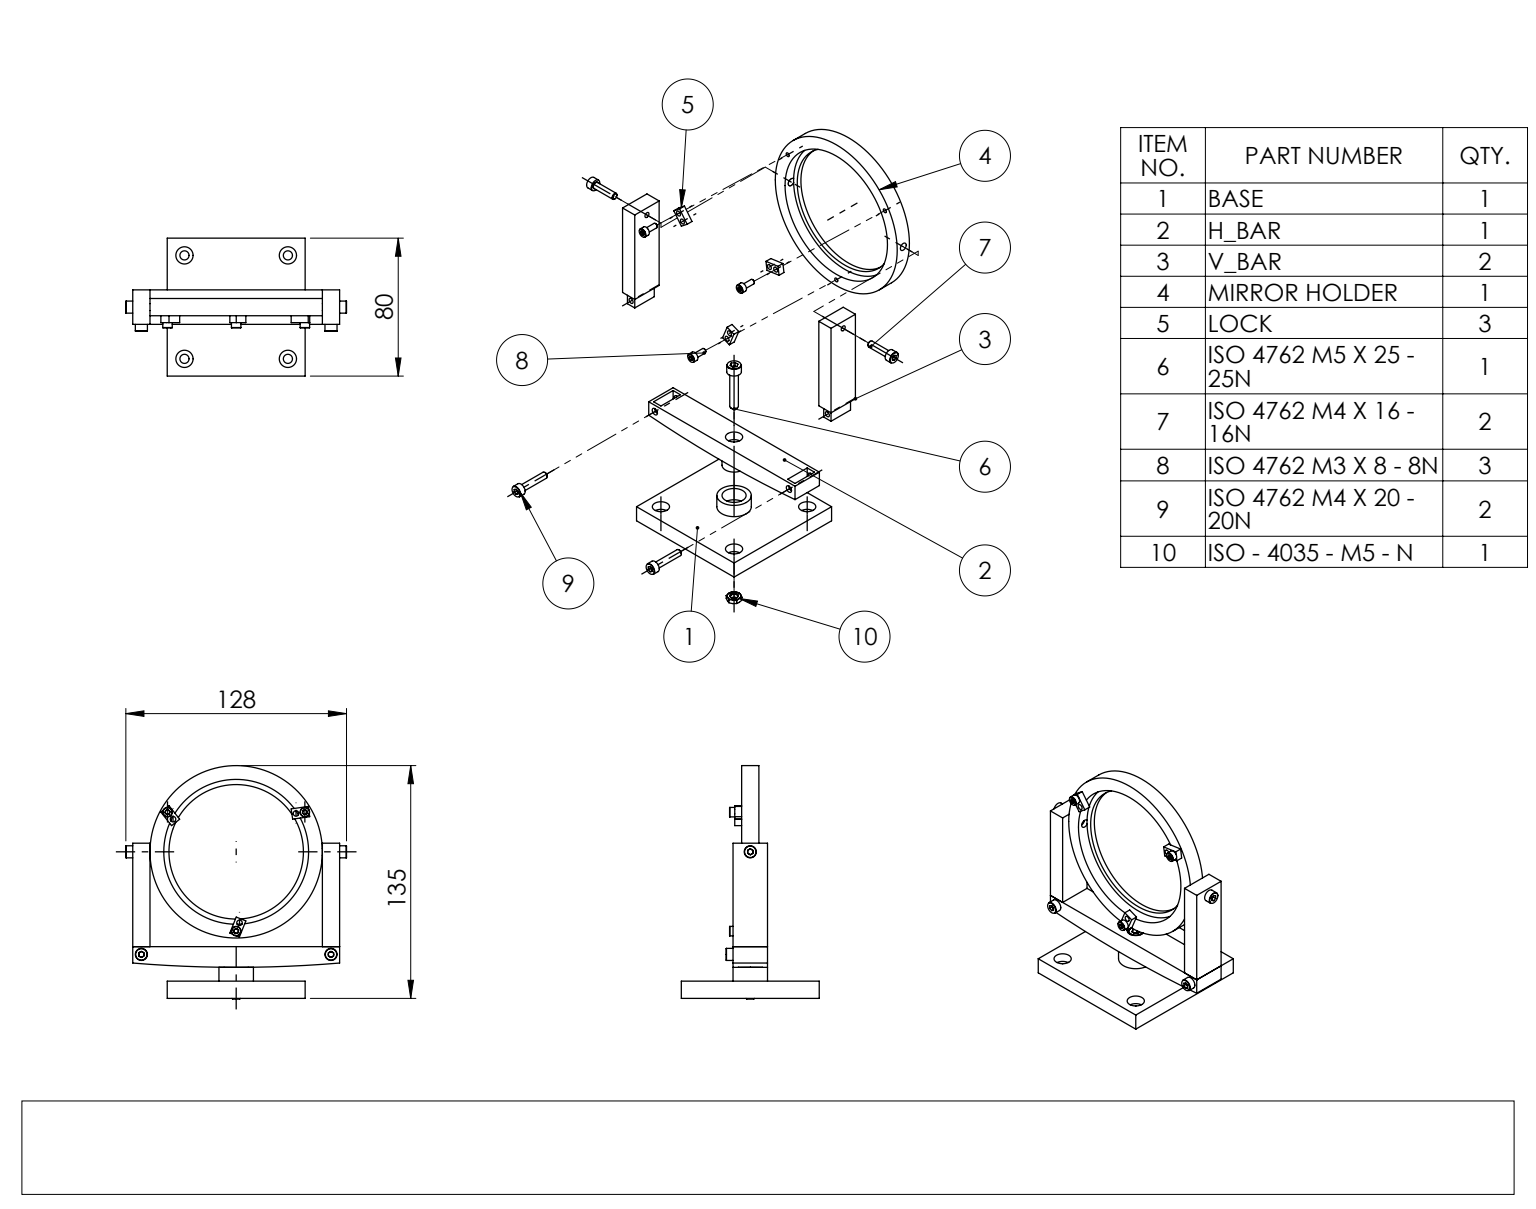
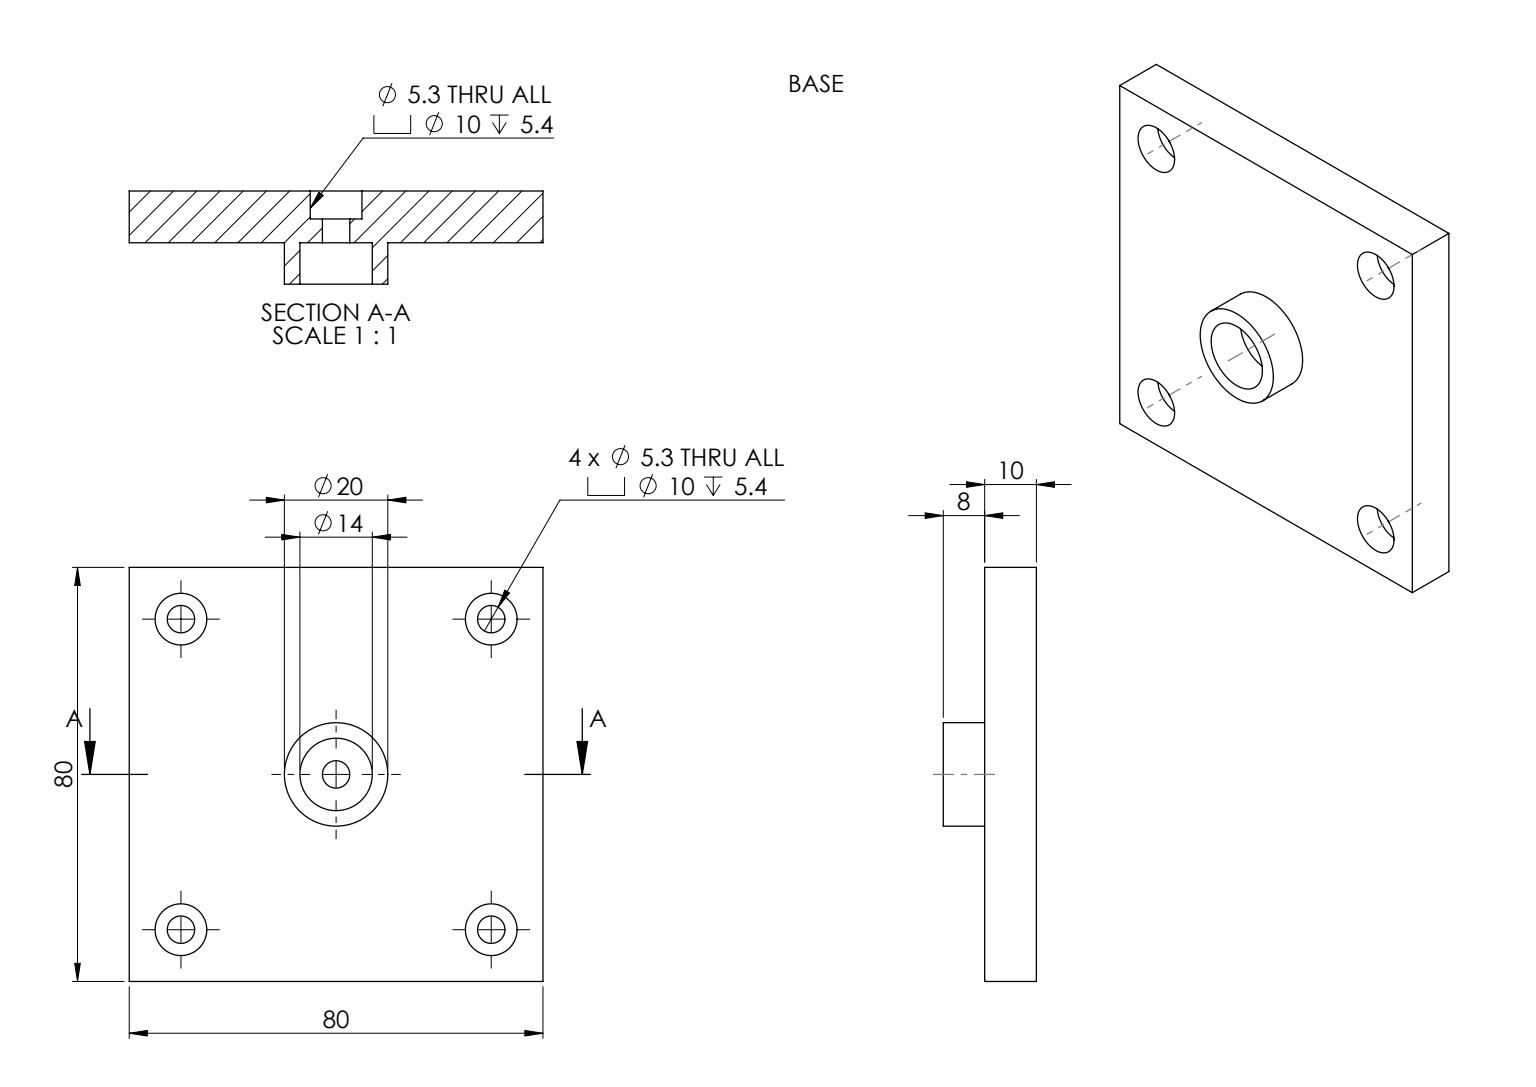
ISO-10303-21;
HEADER;
FILE_DESCRIPTION (('STEP AP214'),
    '1' );
FILE_NAME ('BR-153',
    '2026-10-08T12:12:07',
    ( '' ),
    ( '' ),
    'SwSTEP 2.0',
    'SolidWorks 2026',
    '' );
FILE_SCHEMA (( 'AUTOMOTIVE_DESIGN' ));
ENDSEC;

DATA;
#1 = ORIENTED_EDGE ( 'NONE', *, *, #482, .T. ) ;
#2 = DIRECTION ( 'NONE',  ( -0.000000000000000000, -0.000000000000000000, -1.000000000000000000 ) ) ;
#3 = ORIENTED_EDGE ( 'NONE', *, *, #6998, .T. ) ;
#4 = ORIENTED_EDGE ( 'NONE', *, *, #3995, .T. ) ;
#5 = PRODUCT_DEFINITION_SHAPE ( 'NONE', 'NONE',  #2283 ) ;
#6 = DIRECTION ( 'NONE',  ( -1.000000000000000000, 0.000000000000000000, 0.000000000000000000 ) ) ;
#7 = CARTESIAN_POINT ( 'NONE',  ( -34.99999999999999289, 30.00000000000000711, 10.00000000000000000 ) ) ;
#8 = CARTESIAN_POINT ( 'NONE',  ( 11.00000000000000355, 0.000000000000000000, 1.219500000000000028 ) ) ;
#9 = ADVANCED_BREP_SHAPE_REPRESENTATION ( '', ( #3934, #1587 ), #3111 ) ;
#10 = DIRECTION ( 'NONE',  ( 0.6609621790636541760, 0.7504192147376197441, -8.448647189793598288E-19 ) ) ;
#11 = CIRCLE ( 'NONE', #4655, 3.299999999999999822 ) ;
#12 = B_SPLINE_CURVE_WITH_KNOTS ( 'NONE', 3,
 ( #534, #1149, #5570, #2945, #3074, #6720 ),
 .UNSPECIFIED., .F., .F.,
 ( 4, 2, 4 ),
 ( 0.006456566858647395761, 0.007625406818786665576, 0.008794246778925936259 ),
 .UNSPECIFIED. ) ;
#13 = ORIENTED_EDGE ( 'NONE', *, *, #1918, .T. ) ;
#14 = CARTESIAN_POINT ( 'NONE',  ( 49.97494079589864668, 83.41331875350536507, -1.807471472119508205 ) ) ;
#15 = ORIENTED_EDGE ( 'NONE', *, *, #6393, .F. ) ;
#16 = EDGE_LOOP ( 'NONE', ( #282, #7065, #6159, #322 ) ) ;
#17 = ADVANCED_FACE ( 'NONE', ( #5328 ), #856, .F. ) ;
#18 = CARTESIAN_POINT ( 'NONE',  ( -10.00000000000000000, 0.000000000000000000, 18.00000000000000355 ) ) ;
#19 = CARTESIAN_POINT ( 'NONE',  ( 42.00000000000004263, 84.74554347572708934, -2.399999999999959943 ) ) ;
#20 = DIRECTION ( 'NONE',  ( 0.8191520442889896891, 1.003171929053522158E-16, -0.5735764363510490460 ) ) ;
#21 =( LENGTH_UNIT ( ) NAMED_UNIT ( * ) SI_UNIT ( .MILLI., .METRE. ) );
#22 = CYLINDRICAL_SURFACE ( 'NONE', #7576, 2.399999999999985256 ) ;
#23 = ORIENTED_EDGE ( 'NONE', *, *, #1900, .T. ) ;
#24 = ADVANCED_FACE ( 'NONE', ( #2123 ), #1462, .F. ) ;
#25 = CARTESIAN_POINT ( 'NONE',  ( 0.000000000000000000, 0.000000000000000000, 0.000000000000000000 ) ) ;
#26 = CARTESIAN_POINT ( 'NONE',  ( 0.1999999999999987899, 0.000000000000000000, 0.000000000000000000 ) ) ;
#27 = CARTESIAN_POINT ( 'NONE',  ( 29.99999999999997868, 30.00000000000001421, 10.00000000000000000 ) ) ;
#28 = CARTESIAN_POINT ( 'NONE',  ( 1.300000000000000044, 1.478016689125442484, -1.626303258728256651E-15 ) ) ;
#29 = DIRECTION ( 'NONE',  ( 1.000000000000000000, 0.000000000000000000, 0.000000000000000000 ) ) ;
#30 = CARTESIAN_POINT ( 'NONE',  ( 29.99999999999997868, 30.00000000000001421, 10.00000000000000000 ) ) ;
#31 = VECTOR ( 'NONE', #6228, 1000.000000000000000 ) ;
#32 = EDGE_LOOP ( 'NONE', ( #2251, #1109, #2656, #3323 ) ) ;
#33 = EDGE_CURVE ( 'NONE', #5370, #4266, #4037, .T. ) ;
#34 = FACE_OUTER_BOUND ( 'NONE', #4042, .T. ) ;
#35 = DIRECTION ( 'NONE',  ( 0.000000000000000000, -0.000000000000000000, -1.000000000000000000 ) ) ;
#36 = CARTESIAN_POINT ( 'NONE',  ( -54.99999999999990052, 7.999999999999996447, 17.64999999999876579 ) ) ;
#37 = CARTESIAN_POINT ( 'NONE',  ( 2.649999999999999023, 0.000000000000000000, 20.00000000000000355 ) ) ;
#38 = ORIENTED_EDGE ( 'NONE', *, *, #3972, .T. ) ;
#39 = ORIENTED_EDGE ( 'NONE', *, *, #6953, .F. ) ;
#40 = PLANE ( 'NONE',  #657 ) ;
#41 = EDGE_LOOP ( 'NONE', ( #7482, #4970, #5659, #4712 ) ) ;
#42 = ORIENTED_EDGE ( 'NONE', *, *, #1737, .T. ) ;
#43 = ORIENTED_EDGE ( 'NONE', *, *, #111, .F. ) ;
#44 = CARTESIAN_POINT ( 'NONE',  ( -42.00000000000000711, 85.00000000000046896, 2.399999999999971045 ) ) ;
#45 = DIRECTION ( 'NONE',  ( 1.000000000000000000, 0.000000000000000000, 0.000000000000000000 ) ) ;
#46 = FACE_OUTER_BOUND ( 'NONE', #941, .T. ) ;
#47 = ORIENTED_EDGE ( 'NONE', *, *, #2802, .T. ) ;
#48 = EDGE_CURVE ( 'NONE', #4570, #1158, #4656, .T. ) ;
#49 = ORIENTED_EDGE ( 'NONE', *, *, #6995, .T. ) ;
#50 = EDGE_CURVE ( 'NONE', #5044, #7574, #6013, .T. ) ;
#51 = ORIENTED_EDGE ( 'NONE', *, *, #3552, .T. ) ;
#52 = ADVANCED_FACE ( 'NONE', ( #6515 ), #2195, .F. ) ;
#53 = MECHANICAL_DESIGN_GEOMETRIC_PRESENTATION_REPRESENTATION (  '', ( #5634 ), #3784 ) ;
#54 = CARTESIAN_POINT ( 'NONE',  ( 55.00000000000000000, -8.000000000000001776, -4.499999999999986677 ) ) ;
#55 = CARTESIAN_POINT ( 'NONE',  ( 41.93508307841050708, 82.66544186248239612, -0.5710001583723857133 ) ) ;
#56 = DIRECTION ( 'NONE',  ( 0.000000000000000000, 0.000000000000000000, 1.000000000000000000 ) ) ;
#57 = ORIENTED_EDGE ( 'NONE', *, *, #5357, .F. ) ;
#58 = DIRECTION ( 'NONE',  ( 1.412205397084881070E-17, -2.775557561562891967E-17, -1.000000000000000000 ) ) ;
#59 = DIRECTION ( 'NONE',  ( -1.412205397084881070E-17, 2.775557561562891967E-17, 1.000000000000000000 ) ) ;
#60 = EDGE_CURVE ( 'NONE', #480, #1132, #5248, .T. ) ;
#61 = DIRECTION ( 'NONE',  ( -1.000000000000000000, 0.000000000000000000, 0.000000000000000000 ) ) ;
#62 = FACE_OUTER_BOUND ( 'NONE', #6300, .T. ) ;
#63 = EDGE_CURVE ( 'NONE', #397, #8121, #700, .T. ) ;
#64 =( REPRESENTATION_RELATIONSHIP ('NONE','NONE', #3916, #3059 ) REPRESENTATION_RELATIONSHIP_WITH_TRANSFORMATION ( #3661 )SHAPE_REPRESENTATION_RELATIONSHIP( ) );
#65 = EDGE_LOOP ( 'NONE', ( #3334, #6750, #4812, #6687 ) ) ;
#66 = LINE ( 'NONE', #3278, #5122 ) ;
#67 = FACE_OUTER_BOUND ( 'NONE', #4002, .T. ) ;
#68 = FACE_OUTER_BOUND ( 'NONE', #3488, .T. ) ;
#69 = CYLINDRICAL_SURFACE ( 'NONE', #6742, 1.599999999999992983 ) ;
#70 =( NAMED_UNIT ( * ) SI_UNIT ( $, .STERADIAN. ) SOLID_ANGLE_UNIT ( ) );
#71 = B_SPLINE_CURVE_WITH_KNOTS ( 'NONE', 3,
 ( #3365, #3998, #818, #3718, #2730, #6286, #158, #589, #14, #5859, #6912, #2467, #2700, #6512, #1264, #1222, #4609, #1172, #6467, #3136, #4426, #5671, #1897, #8185, #2045, #5894, #631, #5007, #778, #5278, #552, #5630 ),
 .UNSPECIFIED., .F., .F.,
 ( 4, 2, 2, 2, 2, 2, 2, 2, 2, 2, 2, 2, 2, 2, 2, 4 ),
 ( 0.000000000000000000, 0.0004690358444888099608, 0.0009380716889776199215, 0.001407107533466429774, 0.001876143377955239843, 0.002345179222444049912, 0.002814215066932859548, 0.003752286755910464074, 0.004221322600399265469, 0.004690358444888067732, 0.005159394289376869995, 0.005628430133865671391, 0.006097465978354474521, 0.006566501822843276784, 0.007035537667332079914, 0.007504573511820881310 ),
 .UNSPECIFIED. ) ;
#72 = ORIENTED_EDGE ( 'NONE', *, *, #716, .T. ) ;
#73 = EDGE_LOOP ( 'NONE', ( #3445, #4824, #2962, #715 ) ) ;
#74 = FACE_OUTER_BOUND ( 'NONE', #4146, .T. ) ;
#75 = ORIENTED_EDGE ( 'NONE', *, *, #2802, .F. ) ;
#76 = EDGE_LOOP ( 'NONE', ( #7963, #1978, #1867, #3396 ) ) ;
#77 = AXIS2_PLACEMENT_3D ( 'NONE', #6782, #2260, #420 ) ;
#78 = DIRECTION ( 'NONE',  ( -1.000000000000000000, 0.000000000000000000, 0.000000000000000000 ) ) ;
#79 = DIRECTION ( 'NONE',  ( 0.000000000000000000, -0.5000000000000009992, -0.8660254037844380415 ) ) ;
#80 = DIRECTION ( 'NONE',  ( 0.000000000000000000, -0.000000000000000000, 1.000000000000000000 ) ) ;
#81 = DIRECTION ( 'NONE',  ( 6.123233995736766036E-17, 1.363075293218192124E-18, -1.000000000000000000 ) ) ;
#82 = EDGE_CURVE ( 'NONE', #4888, #7000, #5116, .T. ) ;
#83 = ORIENTED_EDGE ( 'NONE', *, *, #3647, .F. ) ;
#84 = EDGE_CURVE ( 'NONE', #954, #5289, #7760, .T. ) ;
#85 = ORIENTED_EDGE ( 'NONE', *, *, #3347, .T. ) ;
#86 = ORIENTED_EDGE ( 'NONE', *, *, #5141, .F. ) ;
#87 = CARTESIAN_POINT ( 'NONE',  ( 4.000000000000003553, 4.286263797015736595E-16, -3.500000000000000000 ) ) ;
#88 = EDGE_CURVE ( 'NONE', #1891, #7622, #3368, .T. ) ;
#89 = CARTESIAN_POINT ( 'NONE',  ( 41.93506701445378582, 87.33484857940398172, -0.5699281247695300312 ) ) ;
#90 = DIRECTION ( 'NONE',  ( 0.000000000000000000, 0.000000000000000000, 1.000000000000000000 ) ) ;
#91 = SURFACE_SIDE_STYLE ('',( #6493 ) ) ;
#92 =( NAMED_UNIT ( * ) PLANE_ANGLE_UNIT ( ) SI_UNIT ( $, .RADIAN. ) );
#93 = AXIS2_PLACEMENT_3D ( 'NONE', #1716, #4922, #1673 ) ;
#94 =( GEOMETRIC_REPRESENTATION_CONTEXT ( 3 ) GLOBAL_UNCERTAINTY_ASSIGNED_CONTEXT ( ( #5253 ) ) GLOBAL_UNIT_ASSIGNED_CONTEXT ( ( #2108, #1487, #1650 ) ) REPRESENTATION_CONTEXT ( 'NONE', 'WORKASPACE' ) );
#95 = DIRECTION ( 'NONE',  ( -1.000000000000000000, 0.000000000000000000, 7.304098846218136639E-16 ) ) ;
#96 = ADVANCED_FACE ( 'NONE', ( #5364 ), #2158, .T. ) ;
#97 = DIRECTION ( 'NONE',  ( 1.000000000000000000, 0.000000000000000000, 0.000000000000000000 ) ) ;
#98 = FACE_OUTER_BOUND ( 'NONE', #4834, .T. ) ;
#99 = VECTOR ( 'NONE', #2043, 1000.000000000000000 ) ;
#100 = EDGE_CURVE ( 'NONE', #953, #6924, #7257, .T. ) ;
#101 = DIRECTION ( 'NONE',  ( -1.000000000000000000, 0.000000000000000000, 0.000000000000000000 ) ) ;
#102 = VECTOR ( 'NONE', #7211, 1000.000000000000000 ) ;
#103 = CARTESIAN_POINT ( 'NONE',  ( 57.99999999999999289, 7.999999999999996447, 11.99999999999998934 ) ) ;
#104 = VECTOR ( 'NONE', #3751, 1000.000000000000000 ) ;
#105 = ADVANCED_FACE ( 'NONE', ( #1577 ), #6609, .T. ) ;
#106 = ORIENTED_EDGE ( 'NONE', *, *, #2494, .F. ) ;
#107 = DIRECTION ( 'NONE',  ( -1.000000000000000000, -0.000000000000000000, -0.000000000000000000 ) ) ;
#108 = AXIS2_PLACEMENT_3D ( 'NONE', #7357, #7319, #2957 ) ;
#109 = PRESENTATION_STYLE_ASSIGNMENT (( #7641 ) ) ;
#110 = FACE_BOUND ( 'NONE', #6288, .T. ) ;
#111 = EDGE_CURVE ( 'NONE', #2701, #7610, #4070, .T. ) ;
#112 = CONICAL_SURFACE ( 'NONE', #2379, 1.535500000000000087, 1.047197551196590748 ) ;
#113 = DIRECTION ( 'NONE',  ( -1.734723475976806848E-16, 1.000000000000000000, -0.000000000000000000 ) ) ;
#114 = VECTOR ( 'NONE', #3066, 1000.000000000000000 ) ;
#115 = CARTESIAN_POINT ( 'NONE',  ( 2.339468227445713477, 3.268109542640642573, 2.462324777668250297E-15 ) ) ;
#116 = AXIS2_PLACEMENT_3D ( 'NONE', #2904, #405, #2981 ) ;
#117 = VERTEX_POINT ( 'NONE', #5975 ) ;
#118 = VECTOR ( 'NONE', #3051, 1000.000000000000000 ) ;
#119 = ORIENTED_EDGE ( 'NONE', *, *, #7559, .F. ) ;
#120 = VECTOR ( 'NONE', #1322, 1000.000000000000000 ) ;
#121 = CARTESIAN_POINT ( 'NONE',  ( -2.500000000000002220, 3.061616997868386099E-16, -2.700000000000001066 ) ) ;
#122 = EDGE_LOOP ( 'NONE', ( #168, #7429, #374, #2887 ) ) ;
#123 = ORIENTED_EDGE ( 'NONE', *, *, #702, .T. ) ;
#124 = VECTOR ( 'NONE', #3649, 1000.000000000000000 ) ;
#125 = DIRECTION ( 'NONE',  ( 0.000000000000000000, 0.000000000000000000, 1.000000000000000000 ) ) ;
#126 = CARTESIAN_POINT ( 'NONE',  ( 39.00000000000003553, 85.00000000000017053, 2.000000000000043965 ) ) ;
#127 = DIRECTION ( 'NONE',  ( -1.000000000000000000, 0.000000000000000000, 2.065146995210483462E-17 ) ) ;
#128 = AXIS2_PLACEMENT_3D ( 'NONE', #4289, #6814, #1125 ) ;
#129 = DIRECTION ( 'NONE',  ( -3.469446951956349780E-18, -7.554287057009999117E-15, -1.000000000000000000 ) ) ;
#130 = AXIS2_PLACEMENT_3D ( 'NONE', #7551, #5648, #7466 ) ;
#131 = B_SPLINE_CURVE_WITH_KNOTS ( 'NONE', 3,
 ( #1454, #3993, #5161, #1526 ),
 .UNSPECIFIED., .F., .F.,
 ( 4, 4 ),
 ( 2.380737581622003645E-07, 0.002336974151641576375 ),
 .UNSPECIFIED. ) ;
#132 = ORIENTED_EDGE ( 'NONE', *, *, #3473, .T. ) ;
#133 = VECTOR ( 'NONE', #5005, 1000.000000000000000 ) ;
#134 = ORIENTED_EDGE ( 'NONE', *, *, #338, .F. ) ;
#135 = VERTEX_POINT ( 'NONE', #2859 ) ;
#136 = AXIS2_PLACEMENT_3D ( 'NONE', #1715, #4290, #4376 ) ;
#137 = FACE_OUTER_BOUND ( 'NONE', #4836, .T. ) ;
#138 = CARTESIAN_POINT ( 'NONE',  ( 41.93122696811919070, 82.59745623955464566, -0.06342023833154092349 ) ) ;
#139 = DIRECTION ( 'NONE',  ( 0.000000000000000000, 0.000000000000000000, 1.000000000000000000 ) ) ;
#140 =( NAMED_UNIT ( * ) PLANE_ANGLE_UNIT ( ) SI_UNIT ( $, .RADIAN. ) );
#141 = SURFACE_STYLE_USAGE ( .BOTH. , #5841 ) ;
#142 = CARTESIAN_POINT ( 'NONE',  ( 60.00000000000000711, 10.00000000000000000, 19.99999999999998224 ) ) ;
#143 = DIRECTION ( 'NONE',  ( -0.000000000000000000, -0.000000000000000000, 1.000000000000000000 ) ) ;
#144 = CARTESIAN_POINT ( 'NONE',  ( 5.930697612239895941E-15, 38.99999999999999289, -4.999999999999990230 ) ) ;
#145 = LINE ( 'NONE', #2653, #909 ) ;
#146 = CARTESIAN_POINT ( 'NONE',  ( -50.00000000000000711, 85.00000000000009948, -2.399999999999999467 ) ) ;
#147 = EDGE_CURVE ( 'NONE', #4940, #6473, #5403, .T. ) ;
#148 = EDGE_CURVE ( 'NONE', #2318, #1485, #8001, .T. ) ;
#149 = ORIENTED_EDGE ( 'NONE', *, *, #1842, .T. ) ;
#150 = EDGE_CURVE ( 'NONE', #5220, #7241, #7933, .T. ) ;
#151 = DIRECTION ( 'NONE',  ( 0.000000000000000000, 0.000000000000000000, 1.000000000000000000 ) ) ;
#152 = CYLINDRICAL_SURFACE ( 'NONE', #1717, 39.00000000000002132 ) ;
#153 = CARTESIAN_POINT ( 'NONE',  ( -0.6543461111163947352, -4.241015250120822699, -2.560849780464845793 ) ) ;
#154 = DIRECTION ( 'NONE',  ( 1.000000000000000000, 0.000000000000000000, 0.000000000000000000 ) ) ;
#155 = CARTESIAN_POINT ( 'NONE',  ( -50.00000000000000711, 85.00000000000009948, 5.000000000000045297 ) ) ;
#156 = CIRCLE ( 'NONE', #5095, 721.2499999999977263 ) ;
#157 = VERTEX_POINT ( 'NONE', #7474 ) ;
#158 = CARTESIAN_POINT ( 'NONE',  ( 49.98571321592399386, 83.79770962390523437, -2.083050663831888638 ) ) ;
#159 = EDGE_LOOP ( 'NONE', ( #4491, #1533, #7142, #8130 ) ) ;
#160 = ORIENTED_EDGE ( 'NONE', *, *, #1858, .F. ) ;
#161 = AXIS2_PLACEMENT_3D ( 'NONE', #5599, #2306, #1096 ) ;
#162 = ORIENTED_EDGE ( 'NONE', *, *, #3354, .T. ) ;
#163 = DIRECTION ( 'NONE',  ( 0.000000000000000000, 1.000000000000000000, -0.000000000000000000 ) ) ;
#164 = PLANE ( 'NONE',  #4502 ) ;
#165 = CARTESIAN_POINT ( 'NONE',  ( -63.02587731009627703, 153.4828593165325117, 4.999999999999990230 ) ) ;
#166 = VERTEX_POINT ( 'NONE', #1074 ) ;
#167 = EDGE_CURVE ( 'NONE', #3524, #3495, #1661, .T. ) ;
#168 = ORIENTED_EDGE ( 'NONE', *, *, #3674, .T. ) ;
#169 = UNCERTAINTY_MEASURE_WITH_UNIT (LENGTH_MEASURE( 1.000000000000000082E-05 ), #2071, 'distance_accuracy_value', 'NONE');
#170 = EDGE_LOOP ( 'NONE', ( #610, #780, #5868, #1620, #3543 ) ) ;
#171 = FACE_BOUND ( 'NONE', #7717, .T. ) ;
#172 = DIRECTION ( 'NONE',  ( -0.000000000000000000, 1.000000000000000000, 1.224646799147353207E-16 ) ) ;
#173 = CARTESIAN_POINT ( 'NONE',  ( 2.000000000000000000, 1.773042676681340968, -2.276824562219559311E-15 ) ) ;
#174 = EDGE_CURVE ( 'NONE', #7038, #1738, #1989, .T. ) ;
#175 = CARTESIAN_POINT ( 'NONE',  ( -2.000000000000009770, 3.464101615137749057, 0.000000000000000000 ) ) ;
#176 = DIRECTION ( 'NONE',  ( -1.000000000000000000, 0.000000000000000000, 1.412205397084726379E-17 ) ) ;
#177 = CARTESIAN_POINT ( 'NONE',  ( 1.599999999999986988, 42.68016229225776925, 0.000000000000000000 ) ) ;
#178 = CARTESIAN_POINT ( 'NONE',  ( 3.099999999999998757, 1.836970198721030181E-16, -1.500000000000000222 ) ) ;
#179 = EDGE_CURVE ( 'NONE', #2593, #4900, #5449, .T. ) ;
#180 = CARTESIAN_POINT ( 'NONE',  ( -34.99999999999999289, -29.99999999999999289, 4.599999999999997868 ) ) ;
#181 = ADVANCED_FACE ( 'NONE', ( #1112 ), #7964, .F. ) ;
#182 = ORIENTED_EDGE ( 'NONE', *, *, #753, .T. ) ;
#183 = LINE ( 'NONE', #4716, #4981 ) ;
#184 = CARTESIAN_POINT ( 'NONE',  ( 0.000000000000000000, -1.773042676681340524, 1.734723475976807094E-15 ) ) ;
#185 = CARTESIAN_POINT ( 'NONE',  ( 2.500000000000002220, -1.178949249685215417, 2.042000000000002036 ) ) ;
#186 = DIRECTION ( 'NONE',  ( 0.000000000000000000, 0.000000000000000000, 1.000000000000000000 ) ) ;
#187 = EDGE_CURVE ( 'NONE', #4246, #4613, #12, .T. ) ;
#188 = LINE ( 'NONE', #4647, #2150 ) ;
#189 = VERTEX_POINT ( 'NONE', #8093 ) ;
#190 = CARTESIAN_POINT ( 'NONE',  ( 2.500000000000002220, 1.178949249685212086, -2.042000000000002036 ) ) ;
#191 = VERTEX_POINT ( 'NONE', #2408 ) ;
#192 = ORIENTED_EDGE ( 'NONE', *, *, #1370, .F. ) ;
#193 = CARTESIAN_POINT ( 'NONE',  ( 52.00000000000000000, 7.999999999999996447, 19.99999999999998934 ) ) ;
#194 = CARTESIAN_POINT ( 'NONE',  ( -24.99999999999999645, 30.00000000000000711, 10.00000000000000000 ) ) ;
#195 = CARTESIAN_POINT ( 'NONE',  ( -2.060000000000000941, 2.522772406243548923E-16, -0.3080913168122707546 ) ) ;
#196 = ITEM_DEFINED_TRANSFORMATION ( 'NONE', 'NONE', #2967,  #1587 ) ;
#197 = EDGE_CURVE ( 'NONE', #2405, #1419, #5179, .T. ) ;
#198 = ORIENTED_EDGE ( 'NONE', *, *, #4864, .T. ) ;
#199 = ORIENTED_EDGE ( 'NONE', *, *, #8204, .F. ) ;
#200 = ORIENTED_EDGE ( 'NONE', *, *, #5028, .F. ) ;
#201 = EDGE_CURVE ( 'NONE', #2355, #5862, #1579, .T. ) ;
#202 = DIRECTION ( 'NONE',  ( -1.000000000000000000, 0.000000000000000000, 1.032573497605241731E-17 ) ) ;
#203 = CARTESIAN_POINT ( 'NONE',  ( 1.817638007539982281, -6.775366854781982084, 8.002150721412645495 ) ) ;
#204 = FACE_OUTER_BOUND ( 'NONE', #353, .T. ) ;
#205 = AXIS2_PLACEMENT_3D ( 'NONE', #4806, #5391, #4058 ) ;
#206 = AXIS2_PLACEMENT_3D ( 'NONE', #1783, #7378, #1108 ) ;
#207 = ORIENTED_EDGE ( 'NONE', *, *, #7666, .F. ) ;
#208 = DIRECTION ( 'NONE',  ( 0.000000000000000000, 0.000000000000000000, 1.000000000000000000 ) ) ;
#209 = DIRECTION ( 'NONE',  ( -1.000000000000000000, -0.000000000000000000, -0.000000000000000000 ) ) ;
#210 = DIRECTION ( 'NONE',  ( -1.000000000000000000, 0.000000000000000000, 0.000000000000000000 ) ) ;
#211 = CARTESIAN_POINT ( 'NONE',  ( 2.500000000000002220, -1.178949249685215417, 2.042000000000002036 ) ) ;
#212 = DIRECTION ( 'NONE',  ( -1.000000000000000000, -0.000000000000000000, -0.000000000000000000 ) ) ;
#213 = STYLED_ITEM ( 'NONE', ( #3872 ), #6686 ) ;
#214 = ORIENTED_EDGE ( 'NONE', *, *, #5188, .T. ) ;
#215 = DIRECTION ( 'NONE',  ( 0.000000000000000000, 0.000000000000000000, 1.000000000000000000 ) ) ;
#216 = ADVANCED_FACE ( 'NONE', ( #5490 ), #4856, .T. ) ;
#217 = CARTESIAN_POINT ( 'NONE',  ( 4.000000000000000000, 0.000000000000000000, -2.700000000000001066 ) ) ;
#218 = DIRECTION ( 'NONE',  ( 1.000000000000000000, 0.000000000000000000, 0.000000000000000000 ) ) ;
#219 = DIRECTION ( 'NONE',  ( -0.000000000000000000, -0.000000000000000000, 1.000000000000000000 ) ) ;
#220 = EDGE_CURVE ( 'NONE', #3553, #6469, #2177, .T. ) ;
#221 = CARTESIAN_POINT ( 'NONE',  ( 2.678494666091051801, 3.072372537026354156, -0.03421028094653037754 ) ) ;
#222 = EDGE_CURVE ( 'NONE', #3673, #8139, #7510, .T. ) ;
#223 = AXIS2_PLACEMENT_3D ( 'NONE', #6794, #1143, #8202 ) ;
#224 = CARTESIAN_POINT ( 'NONE',  ( 41.97904239022140160, 83.67335008385828132, 2.000000000000015543 ) ) ;
#225 = ORIENTED_EDGE ( 'NONE', *, *, #1635, .F. ) ;
#226 = PLANE ( 'NONE',  #6849 ) ;
#227 = PRODUCT_DEFINITION_CONTEXT ( 'detailed design', #7630, 'design' ) ;
#228 = EDGE_LOOP ( 'NONE', ( #2747, #2923, #3072 ) ) ;
#229 = ORIENTED_EDGE ( 'NONE', *, *, #6061, .F. ) ;
#230 = AXIS2_PLACEMENT_3D ( 'NONE', #1621, #2735, #4150 ) ;
#231 = CIRCLE ( 'NONE', #4093, 50.00000000000002132 ) ;
#232 = AXIS2_PLACEMENT_3D ( 'NONE', #857, #2671, #5216 ) ;
#233 = CARTESIAN_POINT ( 'NONE',  ( -31.74999999999995737, 0.000000000000000000, 0.000000000000000000 ) ) ;
#234 = LINE ( 'NONE', #6015, #2684 ) ;
#235 = PLANE ( 'NONE',  #5820 ) ;
#236 = CARTESIAN_POINT ( 'NONE',  ( -3.000000000000000888, 45.09008114612887397, 4.000000000000000000 ) ) ;
#237 = PRODUCT_CONTEXT ( 'NONE', #7877, 'mechanical' ) ;
#238 = VECTOR ( 'NONE', #7982, 1000.000000000000000 ) ;
#239 = CIRCLE ( 'NONE', #4755, 2.650000000000010125 ) ;
#240 = ORIENTED_EDGE ( 'NONE', *, *, #3379, .F. ) ;
#241 = EDGE_CURVE ( 'NONE', #2831, #8109, #2243, .T. ) ;
#242 = VECTOR ( 'NONE', #527, 1000.000000000000000 ) ;
#243 = ORIENTED_EDGE ( 'NONE', *, *, #3460, .F. ) ;
#244 = VERTEX_POINT ( 'NONE', #4816 ) ;
#245 = AXIS2_PLACEMENT_3D ( 'NONE', #8189, #4513, #2470 ) ;
#246 = DIRECTION ( 'NONE',  ( 1.000000000000000000, 0.000000000000000000, 0.000000000000000000 ) ) ;
#247 = CARTESIAN_POINT ( 'NONE',  ( 6.063862694340463655, -3.504607373393594294, 8.025483085394268912 ) ) ;
#248 = CONICAL_SURFACE ( 'NONE', #3450, 4.000000000000000000, 1.047197551196595855 ) ;
#249 = AXIS2_PLACEMENT_3D ( 'NONE', #6671, #347, #6580 ) ;
#250 = LINE ( 'NONE', #1476, #2497 ) ;
#251 = PLANE ( 'NONE',  #1285 ) ;
#252 = AXIS2_PLACEMENT_3D ( 'NONE', #5711, #1219, #3844 ) ;
#253 = EDGE_CURVE ( 'NONE', #6951, #2122, #5644, .T. ) ;
#254 = DIRECTION ( 'NONE',  ( -1.000000000000000000, -0.000000000000000000, -0.000000000000000000 ) ) ;
#255 = DIRECTION ( 'NONE',  ( 1.412205397084881070E-17, -2.775557561562891967E-17, -1.000000000000000000 ) ) ;
#256 = AXIS2_PLACEMENT_3D ( 'NONE', #3380, #1548, #4591 ) ;
#257 = DIRECTION ( 'NONE',  ( 0.000000000000000000, 0.8660254037844380415, -0.5000000000000009992 ) ) ;
#258 = DIRECTION ( 'NONE',  ( -0.000000000000000000, -1.000000000000000000, -0.000000000000000000 ) ) ;
#259 = EDGE_CURVE ( 'NONE', #2258, #2818, #4701, .T. ) ;
#260 = ORIENTED_EDGE ( 'NONE', *, *, #7666, .T. ) ;
#261 = ORIENTED_EDGE ( 'NONE', *, *, #7341, .T. ) ;
#262 = DIRECTION ( 'NONE',  ( 0.000000000000000000, 0.000000000000000000, -1.000000000000000000 ) ) ;
#263 = CARTESIAN_POINT ( 'NONE',  ( 0.000000000000000000, 0.000000000000000000, 0.000000000000000000 ) ) ;
#264 = CARTESIAN_POINT ( 'NONE',  ( 25.00000000000001421, -29.99999999999997868, 4.599999999999997868 ) ) ;
#265 = CARTESIAN_POINT ( 'NONE',  ( 60.00000000000000711, 9.332579536216795825E-15, 53.34999999999999432 ) ) ;
#266 = CARTESIAN_POINT ( 'NONE',  ( 55.00000000000000000, 8.000000000000000000, -4.499999999999986677 ) ) ;
#267 = FACE_OUTER_BOUND ( 'NONE', #3148, .T. ) ;
#268 = CARTESIAN_POINT ( 'NONE',  ( 0.000000000000000000, 3.275930187719169848E-16, -2.600000000000000089 ) ) ;
#269 = ORIENTED_EDGE ( 'NONE', *, *, #5618, .F. ) ;
#270 = CARTESIAN_POINT ( 'NONE',  ( 0.000000000000000000, 0.000000000000000000, 60.00000000000000000 ) ) ;
#271 = EDGE_CURVE ( 'NONE', #3838, #583, #4171, .T. ) ;
#272 = ORIENTED_EDGE ( 'NONE', *, *, #404, .T. ) ;
#273 = ORIENTED_EDGE ( 'NONE', *, *, #5939, .F. ) ;
#274 = CARTESIAN_POINT ( 'NONE',  ( 0.000000000000000000, 1.478016689125442484, -1.626303258728256651E-15 ) ) ;
#275 = CARTESIAN_POINT ( 'NONE',  ( 4.000000000000003553, 1.935983797701078757, -2.450530693383765612 ) ) ;
#276 = DIRECTION ( 'NONE',  ( 1.000000000000000000, 0.000000000000000000, 0.000000000000000000 ) ) ;
#277 = AXIS2_PLACEMENT_3D ( 'NONE', #6846, #6974, #1289 ) ;
#278 = DIRECTION ( 'NONE',  ( -1.000000000000000000, 0.000000000000000000, 0.000000000000000000 ) ) ;
#279 = DIRECTION ( 'NONE',  ( 0.000000000000000000, 0.8660254037844380415, -0.5000000000000009992 ) ) ;
#280 = SHAPE_DEFINITION_REPRESENTATION ( #4248, #3059 ) ;
#281 = VECTOR ( 'NONE', #2931, 1000.000000000000000 ) ;
#282 = ORIENTED_EDGE ( 'NONE', *, *, #5845, .T. ) ;
#283 = ORIENTED_EDGE ( 'NONE', *, *, #342, .T. ) ;
#284 = ORIENTED_EDGE ( 'NONE', *, *, #776, .T. ) ;
#285 = DIRECTION ( 'NONE',  ( 1.412205397084881070E-17, -2.775557561562891967E-17, -1.000000000000000000 ) ) ;
#286 = CARTESIAN_POINT ( 'NONE',  ( 6.775412730438223896, -1.817364742217071338, 8.031819226609355766 ) ) ;
#287 = DIRECTION ( 'NONE',  ( 1.000000000000000000, 0.000000000000000000, 0.000000000000000000 ) ) ;
#288 = PRODUCT_RELATED_PRODUCT_CATEGORY ( 'part', '', ( #7499 ) ) ;
#289 = PRODUCT_DEFINITION_FORMATION_WITH_SPECIFIED_SOURCE ( 'ANY', '', #1201, .NOT_KNOWN. ) ;
#290 = FILL_AREA_STYLE_COLOUR ( '', #5069 ) ;
#291 = EDGE_CURVE ( 'NONE', #5142, #1419, #574, .T. ) ;
#292 = EDGE_CURVE ( 'NONE', #5760, #2794, #1287, .T. ) ;
#293 = ADVANCED_BREP_SHAPE_REPRESENTATION ( '', ( #1362, #1587 ), #1923 ) ;
#294 = PRESENTATION_LAYER_ASSIGNMENT (  '', '', ( #7478 ) ) ;
#295 = CARTESIAN_POINT ( 'NONE',  ( 2.500000000000002220, 1.768423874527826678, 1.020999999999997687 ) ) ;
#296 = FACE_OUTER_BOUND ( 'NONE', #3886, .T. ) ;
#297 = DIRECTION ( 'NONE',  ( 0.000000000000000000, 0.5000000000000009992, 0.8660254037844380415 ) ) ;
#298 = AXIS2_PLACEMENT_3D ( 'NONE', #7581, #3223, #4423 ) ;
#299 = DIRECTION ( 'NONE',  ( 0.000000000000000000, 0.000000000000000000, -1.000000000000000000 ) ) ;
#300 = ORIENTED_EDGE ( 'NONE', *, *, #63, .T. ) ;
#301 = EDGE_LOOP ( 'NONE', ( #243, #2979, #6327, #8103 ) ) ;
#302 = FACE_BOUND ( 'NONE', #1666, .T. ) ;
#303 = EDGE_CURVE ( 'NONE', #972, #4432, #3116, .T. ) ;
#304 = DIRECTION ( 'NONE',  ( 1.000000000000000000, 0.000000000000000000, 0.000000000000000000 ) ) ;
#305 = AXIS2_PLACEMENT_3D ( 'NONE', #5138, #679, #789 ) ;
#306 = CARTESIAN_POINT ( 'NONE',  ( -41.93238906222609330, 87.38229022169096538, 0.3178396967578642762 ) ) ;
#307 = DIRECTION ( 'NONE',  ( 0.000000000000000000, 1.000000000000000000, -1.320393690296331133E-15 ) ) ;
#308 = CARTESIAN_POINT ( 'NONE',  ( -49.94312129582967685, 82.61555530433810191, -0.3147289805187312162 ) ) ;
#309 = EDGE_CURVE ( 'NONE', #5533, #6468, #2599, .T. ) ;
#310 = FACE_BOUND ( 'NONE', #6643, .T. ) ;
#311 = ORIENTED_EDGE ( 'NONE', *, *, #3355, .T. ) ;
#312 = DIRECTION ( 'NONE',  ( 0.000000000000000000, 0.000000000000000000, 1.000000000000000000 ) ) ;
#313 = CIRCLE ( 'NONE', #3509, 7.000000000000000000 ) ;
#314 = VERTEX_POINT ( 'NONE', #7605 ) ;
#315 = EDGE_LOOP ( 'NONE', ( #5277, #4331 ) ) ;
#316 = DIRECTION ( 'NONE',  ( 1.000000000000000000, 0.000000000000000000, 0.000000000000000000 ) ) ;
#317 = LINE ( 'NONE', #2196, #5299 ) ;
#318 = CARTESIAN_POINT ( 'NONE',  ( 3.999999999999989786, -2.309401076758547777, -2.342734410091827701 ) ) ;
#319 = LINE ( 'NONE', #2908, #3181 ) ;
#320 = SURFACE_SIDE_STYLE ('',( #905 ) ) ;
#321 = ORIENTED_EDGE ( 'NONE', *, *, #7755, .T. ) ;
#322 = ORIENTED_EDGE ( 'NONE', *, *, #4660, .T. ) ;
#323 = ORIENTED_EDGE ( 'NONE', *, *, #6415, .F. ) ;
#324 = CARTESIAN_POINT ( 'NONE',  ( 1.300000000000000044, 1.690103923579304181E-15, 1.280000000000000249 ) ) ;
#325 = EDGE_CURVE ( 'NONE', #2405, #6988, #1374, .T. ) ;
#326 = CYLINDRICAL_SURFACE ( 'NONE', #7568, 2.649999999999999467 ) ;
#327 = CARTESIAN_POINT ( 'NONE',  ( 2.000000000000000000, -0.8865213383406690406, 1.535500000000000975 ) ) ;
#328 = SHAPE_REPRESENTATION_RELATIONSHIP ( 'NONE' , 'NONE' ,  #3059, #9 ) ;
#329 = EDGE_CURVE ( 'NONE', #4266, #3008, #313, .T. ) ;
#330 = ORIENTED_EDGE ( 'NONE', *, *, #3696, .T. ) ;
#331 = DIRECTION ( 'NONE',  ( -0.7071067811865355823, 0.000000000000000000, 0.7071067811865595631 ) ) ;
#332 = CARTESIAN_POINT ( 'NONE',  ( 2.650000000000010125, 3.245314017740498288E-16, 5.400000000000002132 ) ) ;
#333 = FACE_OUTER_BOUND ( 'NONE', #4314, .T. ) ;
#334 = AXIS2_PLACEMENT_3D ( 'NONE', #7679, #2694, #3873 ) ;
#335 = SURFACE_STYLE_USAGE ( .BOTH. , #876 ) ;
#336 = CARTESIAN_POINT ( 'NONE',  ( -4.999999999999993783, 0.000000000000000000, 3.851859888774471706E-31 ) ) ;
#337 = CARTESIAN_POINT ( 'NONE',  ( 55.00000000000000000, -8.000000000000001776, 17.64999999999999858 ) ) ;
#338 = EDGE_CURVE ( 'NONE', #4916, #3085, #3906, .T. ) ;
#339 = ORIENTED_EDGE ( 'NONE', *, *, #6913, .F. ) ;
#340 = EDGE_LOOP ( 'NONE', ( #4876, #7853, #1305 ) ) ;
#341 = CARTESIAN_POINT ( 'NONE',  ( 2.000000000000000000, 1.773042676681340968, -2.276824562219559311E-15 ) ) ;
#342 = EDGE_CURVE ( 'NONE', #1297, #5311, #66, .T. ) ;
#343 = CARTESIAN_POINT ( 'NONE',  ( 1.084202172485504434E-14, 4.618802153517020948, -2.342734410091827701 ) ) ;
#344 = PLANE ( 'NONE',  #4474 ) ;
#345 = CYLINDRICAL_SURFACE ( 'NONE', #7671, 2.500000000000000444 ) ;
#346 = DIRECTION ( 'NONE',  ( 1.000000000000000000, 0.000000000000000000, 0.000000000000000000 ) ) ;
#347 = DIRECTION ( 'NONE',  ( -0.000000000000000000, 1.000000000000000000, -0.000000000000000000 ) ) ;
#348 = CARTESIAN_POINT ( 'NONE',  ( -4.000000000000000000, 2.309401076758496263, -2.700000000000000178 ) ) ;
#349 = ORIENTED_EDGE ( 'NONE', *, *, #6360, .F. ) ;
#350 = LINE ( 'NONE', #2279, #863 ) ;
#351 = ADVANCED_FACE ( 'NONE', ( #5809 ), #6431, .T. ) ;
#352 = ORIENTED_EDGE ( 'NONE', *, *, #4978, .F. ) ;
#353 = EDGE_LOOP ( 'NONE', ( #7067, #4425, #6961, #3331 ) ) ;
#354 = EDGE_CURVE ( 'NONE', #3615, #8148, #1959, .T. ) ;
#355 = VECTOR ( 'NONE', #5353, 1000.000000000000114 ) ;
#356 = DIRECTION ( 'NONE',  ( 0.000000000000000000, -1.000000000000000000, 0.000000000000000000 ) ) ;
#357 = DIRECTION ( 'NONE',  ( 0.000000000000000000, 0.000000000000000000, 1.000000000000000000 ) ) ;
#358 = DIRECTION ( 'NONE',  ( 1.412205397084881070E-17, -2.775557561562891967E-17, -1.000000000000000000 ) ) ;
#359 = AXIS2_PLACEMENT_3D ( 'NONE', #4680, #2767, #7953 ) ;
#360 = DIRECTION ( 'NONE',  ( -0.000000000000000000, 1.467581828789149729E-15, 1.000000000000000000 ) ) ;
#361 = CARTESIAN_POINT ( 'NONE',  ( -58.00000000000006395, -8.000000000000003553, 19.99999999999998934 ) ) ;
#362 = CIRCLE ( 'NONE', #5165, 4.000000000000000888 ) ;
#363 = AXIS2_PLACEMENT_3D ( 'NONE', #6847, #4450, #6938 ) ;
#364 = EDGE_LOOP ( 'NONE', ( #6417, #7648 ) ) ;
#365 = ORIENTED_EDGE ( 'NONE', *, *, #220, .T. ) ;
#366 = VERTEX_POINT ( 'NONE', #4564 ) ;
#367 = CARTESIAN_POINT ( 'NONE',  ( 2.000000000000000000, 0.000000000000000000, 0.000000000000000000 ) ) ;
#368 = AXIS2_PLACEMENT_3D ( 'NONE', #6411, #7765, #5900 ) ;
#369 = CARTESIAN_POINT ( 'NONE',  ( -60.00000000000000000, 10.00000000000000000, 20.00000000000000355 ) ) ;
#370 = CARTESIAN_POINT ( 'NONE',  ( -3.469446951953613006E-15, 0.000000000000000000, 20.00000000000000355 ) ) ;
#371 = CIRCLE ( 'NONE', #3847, 7.000000000000000000 ) ;
#372 = AXIS2_PLACEMENT_3D ( 'NONE', #7047, #966, #5953 ) ;
#373 = AXIS2_PLACEMENT_3D ( 'NONE', #144, #3901, #4524 ) ;
#374 = ORIENTED_EDGE ( 'NONE', *, *, #6408, .F. ) ;
#375 = DIRECTION ( 'NONE',  ( 0.8660254037844352659, -0.5000000000000056621, 0.000000000000000000 ) ) ;
#376 = EDGE_LOOP ( 'NONE', ( #2346, #2970, #7740, #5830, #3828 ) ) ;
#377 = AXIS2_PLACEMENT_3D ( 'NONE', #2206, #6560, #5374 ) ;
#378 = CIRCLE ( 'NONE', #915, 0.2000000000000000944 ) ;
#379 = CYLINDRICAL_SURFACE ( 'NONE', #4378, 2.649999999999999467 ) ;
#380 = LINE ( 'NONE', #2927, #3726 ) ;
#381 = PRODUCT_DEFINITION_SHAPE ( 'NONE', 'NONE',  #8213 ) ;
#382 = CARTESIAN_POINT ( 'NONE',  ( -6.821151181492251858, -1.588688383954758754, 8.032254533892484005 ) ) ;
#383 = UNCERTAINTY_MEASURE_WITH_UNIT (LENGTH_MEASURE( 1.000000000000000082E-05 ), #5531, 'distance_accuracy_value', 'NONE');
#384 = AXIS2_PLACEMENT_3D ( 'NONE', #6730, #6116, #6907 ) ;
#385 = DIRECTION ( 'NONE',  ( -1.000000000000000000, 0.000000000000000000, -0.000000000000000000 ) ) ;
#386 = EDGE_CURVE ( 'NONE', #1419, #3458, #8149, .T. ) ;
#387 = ORIENTED_EDGE ( 'NONE', *, *, #1940, .F. ) ;
#388 = CIRCLE ( 'NONE', #7708, 3.500000000000000000 ) ;
#389 = ORIENTED_EDGE ( 'NONE', *, *, #5878, .F. ) ;
#390 = FACE_OUTER_BOUND ( 'NONE', #5670, .T. ) ;
#391 = DIRECTION ( 'NONE',  ( -0.000000000000000000, -0.000000000000000000, 1.000000000000000000 ) ) ;
#392 = CARTESIAN_POINT ( 'NONE',  ( -41.94721337724058685, 87.11014508430733372, -1.171319538143981820 ) ) ;
#393 = DIRECTION ( 'NONE',  ( 1.000000000000000000, 0.000000000000000000, 0.000000000000000000 ) ) ;
#394 = DIRECTION ( 'NONE',  ( 0.000000000000000000, 0.000000000000000000, 1.000000000000000000 ) ) ;
#395 = CONICAL_SURFACE ( 'NONE', #3069, 2.500000000000002220, 0.9599310885968777018 ) ;
#396 = DIRECTION ( 'NONE',  ( 0.000000000000000000, 0.000000000000000000, 1.000000000000000000 ) ) ;
#397 = VERTEX_POINT ( 'NONE', #3159 ) ;
#398 = EDGE_CURVE ( 'NONE', #2960, #580, #3789, .T. ) ;
#399 = CARTESIAN_POINT ( 'NONE',  ( -3.469446951953613006E-15, 0.000000000000000000, 14.60000000000000142 ) ) ;
#400 = EDGE_CURVE ( 'NONE', #3913, #5044, #2617, .T. ) ;
#401 = ADVANCED_FACE ( 'NONE', ( #1245, #7092 ), #6269, .F. ) ;
#402 = VERTEX_POINT ( 'NONE', #4485 ) ;
#403 = ORIENTED_EDGE ( 'NONE', *, *, #5324, .F. ) ;
#404 = EDGE_CURVE ( 'NONE', #1899, #4446, #4447, .T. ) ;
#405 = DIRECTION ( 'NONE',  ( 1.412205397084881070E-17, -2.775557561562891967E-17, -1.000000000000000000 ) ) ;
#406 = CARTESIAN_POINT ( 'NONE',  ( 1.270137496355039850E-14, 85.00000000000011369, 5.000000000000046185 ) ) ;
#407 = DIRECTION ( 'NONE',  ( -0.000000000000000000, 1.000000000000000000, -0.000000000000000000 ) ) ;
#408 = DIRECTION ( 'NONE',  ( 0.000000000000000000, 0.8660254037844391517, 0.4999999999999991673 ) ) ;
#409 =( NAMED_UNIT ( * ) SI_UNIT ( $, .STERADIAN. ) SOLID_ANGLE_UNIT ( ) );
#410 = ORIENTED_EDGE ( 'NONE', *, *, #5702, .T. ) ;
#411 = EDGE_LOOP ( 'NONE', ( #6737, #422 ) ) ;
#412 = ORIENTED_EDGE ( 'NONE', *, *, #702, .F. ) ;
#413 = DIRECTION ( 'NONE',  ( -1.000000000000000000, -0.000000000000000000, -0.000000000000000000 ) ) ;
#414 = DIRECTION ( 'NONE',  ( -0.000000000000000000, 0.000000000000000000, -1.000000000000000000 ) ) ;
#415 = CARTESIAN_POINT ( 'NONE',  ( -31.74999999999995737, 3.367778697655221012E-16, -2.750000000000000000 ) ) ;
#416 =( NAMED_UNIT ( * ) PLANE_ANGLE_UNIT ( ) SI_UNIT ( $, .RADIAN. ) );
#417 = VECTOR ( 'NONE', #2244, 1000.000000000000000 ) ;
#418 = ORIENTED_EDGE ( 'NONE', *, *, #2740, .T. ) ;
#419 = ADVANCED_FACE ( 'NONE', ( #34 ), #2003, .T. ) ;
#420 = DIRECTION ( 'NONE',  ( 0.000000000000000000, 0.000000000000000000, 1.000000000000000000 ) ) ;
#421 = ORIENTED_EDGE ( 'NONE', *, *, #7234, .F. ) ;
#422 = ORIENTED_EDGE ( 'NONE', *, *, #7110, .F. ) ;
#423 = CARTESIAN_POINT ( 'NONE',  ( 41.98518000931063199, 86.13243788719030647, 2.128825685961691416 ) ) ;
#424 = CARTESIAN_POINT ( 'NONE',  ( -2.500000000000002220, 0.000000000000000000, -2.674599999999998978 ) ) ;
#425 = SURFACE_SIDE_STYLE ('',( #7498 ) ) ;
#426 = CARTESIAN_POINT ( 'NONE',  ( -7.000000000000002665, -0.4626139278909737751, 8.033969604113735841 ) ) ;
#427 = CARTESIAN_POINT ( 'NONE',  ( 5.563937487951679195, 4.272621587589405578, 8.021415735625629040 ) ) ;
#428 = CARTESIAN_POINT ( 'NONE',  ( 50.00000000000002842, 85.15661249647209274, 2.399999999999996803 ) ) ;
#429 = ORIENTED_EDGE ( 'NONE', *, *, #1667, .F. ) ;
#430 = ORIENTED_EDGE ( 'NONE', *, *, #3127, .T. ) ;
#431 = FILL_AREA_STYLE ('',( #5077 ) ) ;
#432 = CARTESIAN_POINT ( 'NONE',  ( -3.344563996438217224, -2.687817229851499068, -0.1586754815285014442 ) ) ;
#433 = LINE ( 'NONE', #7335, #3573 ) ;
#434 = EDGE_CURVE ( 'NONE', #4855, #3946, #6691, .T. ) ;
#435 = CARTESIAN_POINT ( 'NONE',  ( 1.300000000000000044, 0.7390083445627193548, -1.280000000000000693 ) ) ;
#436 =( GEOMETRIC_REPRESENTATION_CONTEXT ( 3 ) GLOBAL_UNCERTAINTY_ASSIGNED_CONTEXT ( ( #3628 ) ) GLOBAL_UNIT_ASSIGNED_CONTEXT ( ( #6999, #3191, #7744 ) ) REPRESENTATION_CONTEXT ( 'NONE', 'WORKASPACE' ) );
#437 = DIRECTION ( 'NONE',  ( 1.000000000000000000, 0.000000000000000000, 0.000000000000000000 ) ) ;
#438 = ADVANCED_FACE ( 'NONE', ( #5350 ), #3256, .T. ) ;
#439 = CARTESIAN_POINT ( 'NONE',  ( 52.00000000000000000, 7.999999999999996447, 19.99999999999998934 ) ) ;
#440 = ORIENTED_EDGE ( 'NONE', *, *, #4363, .T. ) ;
#441 = EDGE_LOOP ( 'NONE', ( #6776, #4989, #6704, #8166, #5130 ) ) ;
#442 = AXIS2_PLACEMENT_3D ( 'NONE', #6325, #1425, #7032 ) ;
#443 = B_SPLINE_CURVE_WITH_KNOTS ( 'NONE', 3,
 ( #7017, #115, #221, #1456, #735, #4569 ),
 .UNSPECIFIED., .F., .F.,
 ( 4, 2, 4 ),
 ( 0.002336974151641576375, 0.003500975885716453226, 0.004664977619791330077 ),
 .UNSPECIFIED. ) ;
#444 = CARTESIAN_POINT ( 'NONE',  ( -7.502679033599690683E-14, -4.618802153517020059, -0.3572655899081733644 ) ) ;
#445 = ADVANCED_FACE ( 'NONE', ( #302, #3325 ), #3433, .F. ) ;
#446 = CARTESIAN_POINT ( 'NONE',  ( -29.99999999999999289, 30.00000000000000711, 1.734723475976807094E-15 ) ) ;
#447 = CARTESIAN_POINT ( 'NONE',  ( 0.000000000000000000, -0.8865213383406721492, -1.535499999999998977 ) ) ;
#448 = PLANE ( 'NONE',  #1317 ) ;
#449 = CARTESIAN_POINT ( 'NONE',  ( 4.000000000000003553, 0.000000000000000000, 3.500000000000000000 ) ) ;
#450 = AXIS2_PLACEMENT_3D ( 'NONE', #1025, #3572, #7430 ) ;
#451 = EDGE_LOOP ( 'NONE', ( #6114, #5624, #2081, #2869 ) ) ;
#452 = VERTEX_POINT ( 'NONE', #6506 ) ;
#453 = ORIENTED_EDGE ( 'NONE', *, *, #6162, .T. ) ;
#454 = ADVANCED_FACE ( 'NONE', ( #5886, #6459 ), #5961, .F. ) ;
#455 = CARTESIAN_POINT ( 'NONE',  ( 0.1999999999999987899, 0.000000000000000000, 0.000000000000000000 ) ) ;
#456 = CARTESIAN_POINT ( 'NONE',  ( 30.00000000000000000, 0.000000000000000000, 2.054999999999993054 ) ) ;
#457 = EDGE_CURVE ( 'NONE', #4563, #191, #2069, .T. ) ;
#458 = CYLINDRICAL_SURFACE ( 'NONE', #3417, 4.999999999999993783 ) ;
#459 = UNCERTAINTY_MEASURE_WITH_UNIT (LENGTH_MEASURE( 1.000000000000000082E-05 ), #722, 'distance_accuracy_value', 'NONE');
#460 = SURFACE_STYLE_FILL_AREA ( #2508 ) ;
#461 = EDGE_LOOP ( 'NONE', ( #4654, #4669, #5460, #5904 ) ) ;
#462 = DIRECTION ( 'NONE',  ( 0.000000000000000000, 0.5000000000000011102, 0.8660254037844379305 ) ) ;
#463 = ORIENTED_EDGE ( 'NONE', *, *, #2563, .T. ) ;
#464 = ADVANCED_FACE ( 'NONE', ( #7171 ), #7293, .T. ) ;
#465 = ORIENTED_EDGE ( 'NONE', *, *, #6394, .T. ) ;
#466 = DIRECTION ( 'NONE',  ( 0.000000000000000000, -1.000000000000000000, 0.000000000000000000 ) ) ;
#467 = CARTESIAN_POINT ( 'NONE',  ( -41.93122500247569917, 82.59742185927619573, -0.06338927685520805155 ) ) ;
#468 =( LENGTH_UNIT ( ) NAMED_UNIT ( * ) SI_UNIT ( .MILLI., .METRE. ) );
#469 = CARTESIAN_POINT ( 'NONE',  ( 30.00000000000001066, -29.99999999999997868, 10.00000000000000000 ) ) ;
#470 = CARTESIAN_POINT ( 'NONE',  ( 4.263933714126141972, 5.556256305342602175, 8.012582018583044530 ) ) ;
#471 = VERTEX_POINT ( 'NONE', #2181 ) ;
#472 = ORIENTED_EDGE ( 'NONE', *, *, #697, .T. ) ;
#473 = VECTOR ( 'NONE', #2777, 1000.000000000000000 ) ;
#474 = DIRECTION ( 'NONE',  ( 0.000000000000000000, 0.000000000000000000, 1.000000000000000000 ) ) ;
#475 = CARTESIAN_POINT ( 'NONE',  ( 3.099999999999998757, 0.000000000000000000, -1.600000000000000311 ) ) ;
#476 = DIRECTION ( 'NONE',  ( -0.000000000000000000, -0.000000000000000000, 1.000000000000000000 ) ) ;
#477 = CARTESIAN_POINT ( 'NONE',  ( 29.99999999999997868, 30.00000000000001421, 4.599999999999997868 ) ) ;
#478 = FACE_OUTER_BOUND ( 'NONE', #6860, .T. ) ;
#479 = VERTEX_POINT ( 'NONE', #3947 ) ;
#480 = VERTEX_POINT ( 'NONE', #2766 ) ;
#481 = CARTESIAN_POINT ( 'NONE',  ( 9.020562075079396891E-14, 10.00000000000000000, 8.000000000000007105 ) ) ;
#482 = EDGE_CURVE ( 'NONE', #954, #7060, #183, .T. ) ;
#483 = CARTESIAN_POINT ( 'NONE',  ( 50.00000000000000000, 9.332579536216795825E-15, 53.34999999999998010 ) ) ;
#484 = CARTESIAN_POINT ( 'NONE',  ( 0.000000000000000000, 0.000000000000000000, 10.00000000000000000 ) ) ;
#485 = EDGE_CURVE ( 'NONE', #5247, #2461, #7128, .T. ) ;
#486 = CARTESIAN_POINT ( 'NONE',  ( 1.274374112546295138E-14, 85.00000000000017053, 2.000000000000043521 ) ) ;
#487 = CARTESIAN_POINT ( 'NONE',  ( 1.300000000000000044, 0.000000000000000000, 0.000000000000000000 ) ) ;
#488 = CARTESIAN_POINT ( 'NONE',  ( 3.345653888883671545, -2.687187980154741140, -0.1391502195351559668 ) ) ;
#489 = ORIENTED_EDGE ( 'NONE', *, *, #82, .F. ) ;
#490 = EDGE_LOOP ( 'NONE', ( #4161, #8112 ) ) ;
#491 = VECTOR ( 'NONE', #6667, 1000.000000000000000 ) ;
#492 = ORIENTED_EDGE ( 'NONE', *, *, #3666, .F. ) ;
#493 = VERTEX_POINT ( 'NONE', #7205 ) ;
#494 = CARTESIAN_POINT ( 'NONE',  ( 0.000000000000000000, -1.178949249685215417, 2.042000000000002036 ) ) ;
#495 = AXIS2_PLACEMENT_3D ( 'NONE', #6230, #4451, #4995 ) ;
#496 = DIRECTION ( 'NONE',  ( -0.000000000000000000, 1.000000000000000000, -0.000000000000000000 ) ) ;
#497 = CARTESIAN_POINT ( 'NONE',  ( -58.00000000000006395, -8.000000000000003553, 11.99999999999998934 ) ) ;
#498 = PRESENTATION_STYLE_ASSIGNMENT (( #2994 ) ) ;
#499 = SHAPE_REPRESENTATION ( 'socket head cap screw_iso_ISO 4762 M5 x 25 - 25N', ( #1587 ), #6006 ) ;
#500 = VECTOR ( 'NONE', #5733, 1000.000000000000000 ) ;
#501 = AXIS2_PLACEMENT_3D ( 'NONE', #1664, #4192, #6723 ) ;
#502 = ORIENTED_EDGE ( 'NONE', *, *, #2182, .F. ) ;
#503 = DIRECTION ( 'NONE',  ( -0.000000000000000000, -0.000000000000000000, 1.000000000000000000 ) ) ;
#504 = ADVANCED_FACE ( 'NONE', ( #5237, #6000 ), #4603, .T. ) ;
#505 = EDGE_CURVE ( 'NONE', #4602, #5524, #983, .T. ) ;
#506 = EDGE_LOOP ( 'NONE', ( #7352, #658 ) ) ;
#507 = ORIENTED_EDGE ( 'NONE', *, *, #4695, .F. ) ;
#508 = CONICAL_SURFACE ( 'NONE', #5176, 1.535500000000000087, 1.047197551196590748 ) ;
#509 = APPLICATION_CONTEXT ( 'automotive_design' ) ;
#510 = AXIS2_PLACEMENT_3D ( 'NONE', #2860, #987, #5527 ) ;
#511 = CIRCLE ( 'NONE', #1453, 1.535500000000000087 ) ;
#512 = CARTESIAN_POINT ( 'NONE',  ( -27.34999999999999076, 30.00000000000000711, 10.00000000000000000 ) ) ;
#513 = CARTESIAN_POINT ( 'NONE',  ( -41.96846535023715319, 83.37031242132569275, -1.766478104244469272 ) ) ;
#514 = DIRECTION ( 'NONE',  ( -0.000000000000000000, -0.000000000000000000, 1.000000000000000000 ) ) ;
#515 = CARTESIAN_POINT ( 'NONE',  ( -3.000000000000000888, 45.09008114612887397, 4.000000000000000000 ) ) ;
#516 = CONICAL_SURFACE ( 'NONE', #4902, 2.041999999999999815, 1.047197551196591858 ) ;
#517 =( GEOMETRIC_REPRESENTATION_CONTEXT ( 3 ) GLOBAL_UNCERTAINTY_ASSIGNED_CONTEXT ( ( #1718 ) ) GLOBAL_UNIT_ASSIGNED_CONTEXT ( ( #4596, #2718, #1440 ) ) REPRESENTATION_CONTEXT ( 'NONE', 'WORKASPACE' ) );
#518 = ORIENTED_EDGE ( 'NONE', *, *, #6030, .F. ) ;
#519 = ORIENTED_EDGE ( 'NONE', *, *, #7020, .F. ) ;
#520 = DIRECTION ( 'NONE',  ( 0.000000000000000000, 0.000000000000000000, 1.000000000000000000 ) ) ;
#521 = AXIS2_PLACEMENT_3D ( 'NONE', #6333, #6448, #1357 ) ;
#522 = CARTESIAN_POINT ( 'NONE',  ( -31.74999999999995737, 0.000000000000000000, 0.000000000000000000 ) ) ;
#523 = FACE_OUTER_BOUND ( 'NONE', #5652, .T. ) ;
#524 = CARTESIAN_POINT ( 'NONE',  ( 2.500000000000002220, 3.469446951953614189E-15, 2.041999999999998483 ) ) ;
#525 = AXIS2_PLACEMENT_3D ( 'NONE', #4973, #3598, #1680 ) ;
#526 = AXIS2_PLACEMENT_3D ( 'NONE', #6005, #4849, #7374 ) ;
#527 = DIRECTION ( 'NONE',  ( 1.412205397084881070E-17, -2.775557561562891967E-17, -1.000000000000000000 ) ) ;
#528 = CARTESIAN_POINT ( 'NONE',  ( 2.500000000000015987, 1.768423874527823347, -1.021000000000001018 ) ) ;
#529 = EDGE_CURVE ( 'NONE', #550, #1966, #3988, .T. ) ;
#530 = PRODUCT_DEFINITION_SHAPE ( 'NONE', 'NONE',  #8210 ) ;
#531 = VERTEX_POINT ( 'NONE', #7902 ) ;
#532 = AXIS2_PLACEMENT_3D ( 'NONE', #3087, #2422, #7488 ) ;
#533 = ORIENTED_EDGE ( 'NONE', *, *, #8046, .T. ) ;
#534 = CARTESIAN_POINT ( 'NONE',  ( -4.000000000000000000, 0.000000000000000000, -2.700000000000000178 ) ) ;
#535 = CARTESIAN_POINT ( 'NONE',  ( 3.999999999999989786, -2.309401076758547777, -2.342734410091827701 ) ) ;
#536 = DIRECTION ( 'NONE',  ( 0.000000000000000000, 0.000000000000000000, 1.000000000000000000 ) ) ;
#537 = DIRECTION ( 'NONE',  ( 0.000000000000000000, -1.000000000000000000, 0.000000000000000000 ) ) ;
#538 = LINE ( 'NONE', #3874, #5170 ) ;
#539 = CARTESIAN_POINT ( 'NONE',  ( 52.00000000000000711, -8.000000000000000000, -8.000000000000000000 ) ) ;
#540 =( GEOMETRIC_REPRESENTATION_CONTEXT ( 3 ) GLOBAL_UNCERTAINTY_ASSIGNED_CONTEXT ( ( #3548 ) ) GLOBAL_UNIT_ASSIGNED_CONTEXT ( ( #3306, #2837, #2061 ) ) REPRESENTATION_CONTEXT ( 'NONE', 'WORKASPACE' ) );
#541 = ORIENTED_EDGE ( 'NONE', *, *, #8079, .F. ) ;
#542 = CIRCLE ( 'NONE', #6772, 2.149999999999995470 ) ;
#543 = EDGE_LOOP ( 'NONE', ( #6932, #3498, #8131, #4980, #1347 ) ) ;
#544 = EDGE_LOOP ( 'NONE', ( #2163, #4537, #4576, #1786, #8039 ) ) ;
#545 = EDGE_LOOP ( 'NONE', ( #3135, #132, #1061, #2329, #6550 ) ) ;
#546 = CARTESIAN_POINT ( 'NONE',  ( 4.200000000000001954, 2.449293598294707893E-16, -2.000000000000000888 ) ) ;
#547 = FACE_OUTER_BOUND ( 'NONE', #4009, .T. ) ;
#548 = LINE ( 'NONE', #1806, #3702 ) ;
#549 = EDGE_CURVE ( 'NONE', #1740, #1171, #5269, .T. ) ;
#550 = VERTEX_POINT ( 'NONE', #2722 ) ;
#551 = EDGE_CURVE ( 'NONE', #4688, #1969, #7750, .T. ) ;
#552 = CARTESIAN_POINT ( 'NONE',  ( 50.00000000000001421, 84.84335183244012057, 2.399999999999947509 ) ) ;
#553 = EDGE_LOOP ( 'NONE', ( #5009, #47, #1841 ) ) ;
#554 = VERTEX_POINT ( 'NONE', #4026 ) ;
#555 = CARTESIAN_POINT ( 'NONE',  ( 60.00000000000000711, 9.332579536216795825E-15, 54.99999999999997868 ) ) ;
#556 = EDGE_CURVE ( 'NONE', #3047, #4432, #4306, .T. ) ;
#557 = CARTESIAN_POINT ( 'NONE',  ( -41.93910753963083948, 82.73888917238660667, -0.8146863085833027096 ) ) ;
#558 = PLANE ( 'NONE',  #3293 ) ;
#559 = AXIS2_PLACEMENT_3D ( 'NONE', #4730, #358, #1076 ) ;
#560 = FILL_AREA_STYLE ('',( #1138 ) ) ;
#561 = DIRECTION ( 'NONE',  ( -0.000000000000000000, -0.000000000000000000, 1.000000000000000000 ) ) ;
#562 = AXIS2_PLACEMENT_3D ( 'NONE', #5807, #845, #6662 ) ;
#563 = ORIENTED_EDGE ( 'NONE', *, *, #7710, .T. ) ;
#564 = ORIENTED_EDGE ( 'NONE', *, *, #5523, .T. ) ;
#565 = CYLINDRICAL_SURFACE ( 'NONE', #881, 2.650000000000003020 ) ;
#566 = DIRECTION ( 'NONE',  ( -1.000000000000000000, -0.000000000000000000, -0.000000000000000000 ) ) ;
#567 = CARTESIAN_POINT ( 'NONE',  ( 2.500000000000002220, 2.357898499370434386, -3.469446951953614189E-15 ) ) ;
#568 = CARTESIAN_POINT ( 'NONE',  ( 4.000000000000000000, 0.000000000000000000, 0.000000000000000000 ) ) ;
#569 = CARTESIAN_POINT ( 'NONE',  ( 0.000000000000000000, 1.773042676681340968, -2.276824562219559311E-15 ) ) ;
#570 = PRODUCT_DEFINITION_FORMATION_WITH_SPECIFIED_SOURCE ( 'ANY', '', #3129, .NOT_KNOWN. ) ;
#571 = DIRECTION ( 'NONE',  ( 0.000000000000000000, -1.000000000000000000, 1.222984857324291014E-15 ) ) ;
#572 = EDGE_CURVE ( 'NONE', #954, #5018, #5312, .T. ) ;
#573 = ORIENTED_EDGE ( 'NONE', *, *, #2075, .F. ) ;
#574 = LINE ( 'NONE', #7718, #7494 ) ;
#575 = LINE ( 'NONE', #3747, #3853 ) ;
#576 = CARTESIAN_POINT ( 'NONE',  ( 0.000000000000000000, 0.000000000000000000, 0.000000000000000000 ) ) ;
#577 = FACE_OUTER_BOUND ( 'NONE', #3634, .T. ) ;
#578 = CARTESIAN_POINT ( 'NONE',  ( 49.94601516505094452, 87.32303837806216507, 0.6228612347032452812 ) ) ;
#579 = EDGE_LOOP ( 'NONE', ( #6634, #3876, #4463, #3342 ) ) ;
#580 = VERTEX_POINT ( 'NONE', #4679 ) ;
#581 = CARTESIAN_POINT ( 'NONE',  ( 10.71950000000001424, 0.000000000000000000, 0.000000000000000000 ) ) ;
#582 = PRODUCT_DEFINITION_CONTEXT ( 'detailed design', #6602, 'design' ) ;
#583 = VERTEX_POINT ( 'NONE', #883 ) ;
#584 = ORIENTED_EDGE ( 'NONE', *, *, #7801, .T. ) ;
#585 = FACE_OUTER_BOUND ( 'NONE', #4794, .T. ) ;
#586 = FACE_OUTER_BOUND ( 'NONE', #8062, .T. ) ;
#587 = CARTESIAN_POINT ( 'NONE',  ( 0.000000000000000000, 0.8865213383406685965, -1.535500000000000753 ) ) ;
#588 = EDGE_LOOP ( 'NONE', ( #3671, #2915, #1768, #4961 ) ) ;
#589 = CARTESIAN_POINT ( 'NONE',  ( 49.97875682971463362, 83.53682071867390846, -1.908850074583744671 ) ) ;
#590 = VERTEX_POINT ( 'NONE', #6040 ) ;
#591 = VECTOR ( 'NONE', #2144, 1000.000000000000000 ) ;
#592 = ORIENTED_EDGE ( 'NONE', *, *, #7163, .F. ) ;
#593 = EDGE_CURVE ( 'NONE', #1776, #4324, #8006, .T. ) ;
#594 = ADVANCED_FACE ( 'NONE', ( #2269 ), #7951, .F. ) ;
#595 = FACE_BOUND ( 'NONE', #8029, .T. ) ;
#596 = EDGE_CURVE ( 'NONE', #8175, #5459, #6549, .T. ) ;
#597 = CARTESIAN_POINT ( 'NONE',  ( -41.96116023364841396, 83.19196313526902031, -1.583454828100236522 ) ) ;
#598 = DIRECTION ( 'NONE',  ( 1.000000000000000000, 0.000000000000000000, 0.000000000000000000 ) ) ;
#599 =( LENGTH_UNIT ( ) NAMED_UNIT ( * ) SI_UNIT ( .MILLI., .METRE. ) );
#600 = PRODUCT ( 'lock', 'lock', '', ( #237 ) ) ;
#601 = DIRECTION ( 'NONE',  ( 1.000000000000000000, 2.775557561562890365E-16, -1.734723475976806478E-17 ) ) ;
#602 = FACE_OUTER_BOUND ( 'NONE', #1472, .T. ) ;
#603 = EDGE_LOOP ( 'NONE', ( #3185, #4958, #6458, #2037 ) ) ;
#604 = VERTEX_POINT ( 'NONE', #1255 ) ;
#605 = FACE_OUTER_BOUND ( 'NONE', #2156, .T. ) ;
#606 = CARTESIAN_POINT ( 'NONE',  ( 2.000000000000000000, -0.8865213383406690406, 1.535500000000000975 ) ) ;
#607 = DIRECTION ( 'NONE',  ( -0.000000000000000000, -0.000000000000000000, -1.000000000000000000 ) ) ;
#608 = DIRECTION ( 'NONE',  ( -1.000000000000000000, 0.000000000000000000, 0.000000000000000000 ) ) ;
#609 = LINE ( 'NONE', #3113, #6717 ) ;
#610 = ORIENTED_EDGE ( 'NONE', *, *, #4018, .T. ) ;
#611 = B_SPLINE_CURVE_WITH_KNOTS ( 'NONE', 3,
 ( #7772, #6525, #3415, #4045, #1545, #3464 ),
 .UNSPECIFIED., .F., .F.,
 ( 4, 2, 4 ),
 ( 1.267684120349605325E-16, 0.0006999373991970426947, 0.001399874798393958755 ),
 .UNSPECIFIED. ) ;
#612 = CARTESIAN_POINT ( 'NONE',  ( 2.000000000000000000, 1.773042676681340968, -2.276824562219559311E-15 ) ) ;
#613 = CARTESIAN_POINT ( 'NONE',  ( -39.99999999999999289, -39.99999999999999289, 0.000000000000000000 ) ) ;
#614 = CARTESIAN_POINT ( 'NONE',  ( 2.039008344562727615, -1.214068345727601445E-18, 0.000000000000000000 ) ) ;
#615 = LINE ( 'NONE', #8136, #2509 ) ;
#616 = CARTESIAN_POINT ( 'NONE',  ( -1.600000000000010969, 42.68016229225776925, 0.000000000000000000 ) ) ;
#617 = VECTOR ( 'NONE', #6433, 1000.000000000000114 ) ;
#618 = AXIS2_PLACEMENT_3D ( 'NONE', #4404, #7425, #6266 ) ;
#619 = EDGE_LOOP ( 'NONE', ( #2495, #2179, #7102, #6725 ) ) ;
#620 = EDGE_CURVE ( 'NONE', #2013, #3227, #3446, .T. ) ;
#621 = EDGE_CURVE ( 'NONE', #5625, #2558, #2116, .T. ) ;
#622 = ORIENTED_EDGE ( 'NONE', *, *, #7733, .F. ) ;
#623 = LINE ( 'NONE', #7572, #7694 ) ;
#624 = ORIENTED_EDGE ( 'NONE', *, *, #3897, .T. ) ;
#625 = ORIENTED_EDGE ( 'NONE', *, *, #147, .F. ) ;
#626 = CARTESIAN_POINT ( 'NONE',  ( -41.98522237648275279, 83.86890273273840535, 2.129714952619055524 ) ) ;
#627 = CARTESIAN_POINT ( 'NONE',  ( -52.00000000000006395, 7.999999999999996447, 19.99999999999998934 ) ) ;
#628 = CARTESIAN_POINT ( 'NONE',  ( -3.469446951953613006E-15, 0.000000000000000000, 1.040834085586084257E-14 ) ) ;
#629 = CARTESIAN_POINT ( 'NONE',  ( 76.95406866870810347, 129.3585242258750725, 4.999999999999992895 ) ) ;
#630 = ORIENTED_EDGE ( 'NONE', *, *, #4013, .F. ) ;
#631 = CARTESIAN_POINT ( 'NONE',  ( 49.98889375043669503, 83.93620601285596194, 2.157108981641731038 ) ) ;
#632 = AXIS2_PLACEMENT_3D ( 'NONE', #7048, #58, #176 ) ;
#633 = ORIENTED_EDGE ( 'NONE', *, *, #8107, .F. ) ;
#634 = ADVANCED_FACE ( 'NONE', ( #74 ), #4574, .F. ) ;
#635 = ORIENTED_EDGE ( 'NONE', *, *, #1241, .F. ) ;
#636 = AXIS2_PLACEMENT_3D ( 'NONE', #4081, #799, #139 ) ;
#637 = DIRECTION ( 'NONE',  ( -0.000000000000000000, -0.000000000000000000, 1.000000000000000000 ) ) ;
#638 = CARTESIAN_POINT ( 'NONE',  ( 41.98256188053848348, 83.77272253665795176, -2.078089480949315782 ) ) ;
#639 = CARTESIAN_POINT ( 'NONE',  ( -3.469446951953613006E-15, 0.000000000000000000, 20.00000000000000355 ) ) ;
#640 = VECTOR ( 'NONE', #5019, 1000.000000000000000 ) ;
#641 = DIRECTION ( 'NONE',  ( -1.000000000000000000, -0.000000000000000000, -0.000000000000000000 ) ) ;
#642 = VECTOR ( 'NONE', #6144, 1000.000000000000000 ) ;
#643 = EDGE_CURVE ( 'NONE', #6632, #2779, #3879, .T. ) ;
#644 = CLOSED_SHELL ( 'NONE', ( #6319, #3004, #4176, #1665, #6143, #3927, #6537, #4016, #4322, #2033, #4212, #216, #7611, #5799, #3720, #3409, #351, #4075, #5766, #1524, #4733, #1050, #181, #5566, #5341, #1901, #3631 ) ) ;
#645 = VECTOR ( 'NONE', #1238, 1000.000000000000114 ) ;
#646 = AXIS2_PLACEMENT_3D ( 'NONE', #7732, #7883, #5249 ) ;
#647 = ORIENTED_EDGE ( 'NONE', *, *, #7062, .F. ) ;
#648 = CARTESIAN_POINT ( 'NONE',  ( 3.000000000000002665, 0.000000000000000000, 0.000000000000000000 ) ) ;
#649 = CARTESIAN_POINT ( 'NONE',  ( 30.00000000000000000, 0.000000000000000000, 2.054999999999993054 ) ) ;
#650 = DIRECTION ( 'NONE',  ( 1.000000000000000000, 0.000000000000000000, 0.000000000000000000 ) ) ;
#651 = DIRECTION ( 'NONE',  ( 0.000000000000000000, -0.8660254037844391517, -0.4999999999999992784 ) ) ;
#652 = VECTOR ( 'NONE', #7598, 1000.000000000000000 ) ;
#653 = AXIS2_PLACEMENT_3D ( 'NONE', #5260, #6029, #840 ) ;
#654 = AXIS2_PLACEMENT_3D ( 'NONE', #1822, #7421, #1144 ) ;
#655 = FACE_OUTER_BOUND ( 'NONE', #553, .T. ) ;
#656 = CARTESIAN_POINT ( 'NONE',  ( -50.00000000000000000, 85.31712395750685118, 2.400000000000064748 ) ) ;
#657 = AXIS2_PLACEMENT_3D ( 'NONE', #2591, #1967, #4493 ) ;
#658 = ORIENTED_EDGE ( 'NONE', *, *, #5836, .T. ) ;
#659 = CIRCLE ( 'NONE', #7419, 42.00000000000002132 ) ;
#660 = DIRECTION ( 'NONE',  ( -0.000000000000000000, 1.000000000000000000, -0.000000000000000000 ) ) ;
#661 = VECTOR ( 'NONE', #6389, 1000.000000000000000 ) ;
#662 = CARTESIAN_POINT ( 'NONE',  ( 0.000000000000000000, 2.357898499370434386, -3.469446951953614189E-15 ) ) ;
#663 = CARTESIAN_POINT ( 'NONE',  ( 2.500000000000002220, -1.768423874527823347, 1.021000000000001018 ) ) ;
#664 = CARTESIAN_POINT ( 'NONE',  ( -54.99999999999990052, 10.00000000000000000, 13.34999999999877218 ) ) ;
#665 = EDGE_CURVE ( 'NONE', #554, #1216, #623, .T. ) ;
#666 = CARTESIAN_POINT ( 'NONE',  ( 49.97864901397263537, 86.46689848149799218, -1.906053348878814724 ) ) ;
#667 = EDGE_CURVE ( 'NONE', #3060, #2355, #3891, .T. ) ;
#668 = EDGE_LOOP ( 'NONE', ( #7988, #3759, #463, #418 ) ) ;
#669 = EDGE_CURVE ( 'NONE', #6853, #3935, #3755, .T. ) ;
#670 = AXIS2_PLACEMENT_3D ( 'NONE', #1126, #3587, #2375 ) ;
#671 = EDGE_LOOP ( 'NONE', ( #7354, #3474, #1161, #4159 ) ) ;
#672 = DIRECTION ( 'NONE',  ( 0.000000000000000000, 0.4999999999999990008, -0.8660254037844391517 ) ) ;
#673 = ORIENTED_EDGE ( 'NONE', *, *, #2621, .F. ) ;
#674 = ORIENTED_EDGE ( 'NONE', *, *, #5759, .F. ) ;
#675 = CIRCLE ( 'NONE', #1739, 2.649999999999995914 ) ;
#676 = DIRECTION ( 'NONE',  ( 1.000000000000000000, 0.000000000000000000, 0.000000000000000000 ) ) ;
#677 = DIRECTION ( 'NONE',  ( -1.000000000000000000, -0.000000000000000000, -0.000000000000000000 ) ) ;
#678 = CARTESIAN_POINT ( 'NONE',  ( 0.000000000000000000, 0.000000000000000000, 0.000000000000000000 ) ) ;
#679 = DIRECTION ( 'NONE',  ( 0.000000000000000000, 0.000000000000000000, 1.000000000000000000 ) ) ;
#680 = VECTOR ( 'NONE', #7941, 1000.000000000000000 ) ;
#681 = ORIENTED_EDGE ( 'NONE', *, *, #259, .T. ) ;
#682 = ORIENTED_EDGE ( 'NONE', *, *, #4050, .T. ) ;
#683 = VERTEX_POINT ( 'NONE', #121 ) ;
#684 = DIRECTION ( 'NONE',  ( 0.000000000000000000, -1.000000000000000000, 0.000000000000000000 ) ) ;
#685 = CARTESIAN_POINT ( 'NONE',  ( 41.95055335361874427, 82.96164397218471720, 1.273332678597350442 ) ) ;
#686 = CARTESIAN_POINT ( 'NONE',  ( 39.00000000000003553, 85.00000000000017053, 5.000000000000047073 ) ) ;
#687 = EDGE_CURVE ( 'NONE', #3935, #4267, #2668, .T. ) ;
#688 = DIRECTION ( 'NONE',  ( 1.000000000000000000, 0.000000000000000000, 0.000000000000000000 ) ) ;
#689 = ORIENTED_EDGE ( 'NONE', *, *, #2432, .F. ) ;
#690 = CARTESIAN_POINT ( 'NONE',  ( -29.99999999999999289, 30.00000000000000711, 4.599999999999997868 ) ) ;
#691 = CARTESIAN_POINT ( 'NONE',  ( -39.99999999999999289, -39.99999999999999289, 10.00000000000000000 ) ) ;
#692 = PLANE ( 'NONE',  #3596 ) ;
#693 = CARTESIAN_POINT ( 'NONE',  ( -49.95346081399732441, 87.15763333356271403, 1.062739361928057402 ) ) ;
#694 = VECTOR ( 'NONE', #4778, 1000.000000000000114 ) ;
#695 = EDGE_LOOP ( 'NONE', ( #85, #6665, #2157, #3298, #410 ) ) ;
#696 = CARTESIAN_POINT ( 'NONE',  ( -50.00000000000000711, 85.00000000000009948, 5.000000000000047073 ) ) ;
#697 = EDGE_CURVE ( 'NONE', #1740, #2560, #1589, .T. ) ;
#698 = CARTESIAN_POINT ( 'NONE',  ( -2.649999999999998579, 3.245314017740484976E-16, 1.040834085586084257E-14 ) ) ;
#699 = DIRECTION ( 'NONE',  ( 1.000000000000000000, 0.000000000000000000, 0.000000000000000000 ) ) ;
#700 = B_SPLINE_CURVE_WITH_KNOTS ( 'NONE', 3,
 ( #7879, #7842, #823, #986, #6552, #4728 ),
 .UNSPECIFIED., .F., .F.,
 ( 4, 2, 4 ),
 ( 0.002336974151641522165, 0.003500975885716454527, 0.004664977619791387323 ),
 .UNSPECIFIED. ) ;
#701 = CARTESIAN_POINT ( 'NONE',  ( -2.000000000000009770, 3.464101615137749057, -2.700000000000001066 ) ) ;
#702 = EDGE_CURVE ( 'NONE', #4465, #4618, #5706, .T. ) ;
#703 = CARTESIAN_POINT ( 'NONE',  ( -49.97494079589861826, 83.41331875350518033, 1.807471472119332567 ) ) ;
#704 = EDGE_LOOP ( 'NONE', ( #7531, #5984, #1710, #635 ) ) ;
#705 = EDGE_LOOP ( 'NONE', ( #7620, #3737, #5363, #7417 ) ) ;
#706 = EDGE_CURVE ( 'NONE', #583, #3838, #786, .T. ) ;
#707 = DIRECTION ( 'NONE',  ( 1.000000000000000000, 0.000000000000000000, 0.000000000000000000 ) ) ;
#708 = VERTEX_POINT ( 'NONE', #1382 ) ;
#709 = EDGE_LOOP ( 'NONE', ( #7570, #5169, #7796, #3889 ) ) ;
#710 = DIRECTION ( 'NONE',  ( 0.000000000000000000, 0.000000000000000000, -1.000000000000000000 ) ) ;
#711 = LINE ( 'NONE', #1935, #3202 ) ;
#712 = DIRECTION ( 'NONE',  ( 1.000000000000000000, -0.000000000000000000, -0.000000000000000000 ) ) ;
#713 = CARTESIAN_POINT ( 'NONE',  ( 0.000000000000000000, 26.01196202519846068, 0.000000000000000000 ) ) ;
#714 = ORIENTED_EDGE ( 'NONE', *, *, #6444, .T. ) ;
#715 = ORIENTED_EDGE ( 'NONE', *, *, #2234, .T. ) ;
#716 = EDGE_CURVE ( 'NONE', #4997, #7730, #6980, .T. ) ;
#717 = ORIENTED_EDGE ( 'NONE', *, *, #2095, .F. ) ;
#718 = EDGE_CURVE ( 'NONE', #6876, #5247, #3796, .T. ) ;
#719 = CARTESIAN_POINT ( 'NONE',  ( 32.65000000000000568, -29.99999999999997868, 1.734723475976807094E-15 ) ) ;
#720 = CARTESIAN_POINT ( 'NONE',  ( 41.97904239022140160, 83.67335008385828132, 2.000000000000015543 ) ) ;
#721 = CARTESIAN_POINT ( 'NONE',  ( -59.99999999999999289, 85.00000000000045475, -1.387778780781445676E-14 ) ) ;
#722 =( LENGTH_UNIT ( ) NAMED_UNIT ( * ) SI_UNIT ( .MILLI., .METRE. ) );
#723 = SURFACE_STYLE_USAGE ( .BOTH. , #1946 ) ;
#724 = AXIS2_PLACEMENT_3D ( 'NONE', #6540, #847, #215 ) ;
#725 = EDGE_CURVE ( 'NONE', #4369, #7382, #3169, .T. ) ;
#726 = FACE_OUTER_BOUND ( 'NONE', #4926, .T. ) ;
#727 = DIRECTION ( 'NONE',  ( -0.5000000000000061062, 1.060575238724902601E-16, -0.8660254037844351549 ) ) ;
#728 = CARTESIAN_POINT ( 'NONE',  ( 32.65000000000000568, -29.99999999999997868, 4.599999999999997868 ) ) ;
#729 = FACE_OUTER_BOUND ( 'NONE', #7926, .T. ) ;
#730 = ORIENTED_EDGE ( 'NONE', *, *, #457, .F. ) ;
#731 = DIRECTION ( 'NONE',  ( -1.000000000000000000, -0.000000000000000000, -0.000000000000000000 ) ) ;
#732 = CARTESIAN_POINT ( 'NONE',  ( 1.274374112546295138E-14, 85.00000000000017053, 2.000000000000043521 ) ) ;
#733 = LINE ( 'NONE', #185, #5672 ) ;
#734 = LINE ( 'NONE', #5965, #7798 ) ;
#735 = CARTESIAN_POINT ( 'NONE',  ( 3.673643420401901505, 2.497823135841253706, -0.2484800633749944254 ) ) ;
#736 = ORIENTED_EDGE ( 'NONE', *, *, #147, .T. ) ;
#737 = ORIENTED_EDGE ( 'NONE', *, *, #4756, .F. ) ;
#738 = ADVANCED_FACE ( 'NONE', ( #7614 ), #40, .T. ) ;
#739 = DIRECTION ( 'NONE',  ( -0.000000000000000000, -0.000000000000000000, 1.000000000000000000 ) ) ;
#740 = ORIENTED_EDGE ( 'NONE', *, *, #1500, .F. ) ;
#741 = VERTEX_POINT ( 'NONE', #1345 ) ;
#742 = VECTOR ( 'NONE', #4927, 1000.000000000000000 ) ;
#743 = DIRECTION ( 'NONE',  ( 0.000000000000000000, 0.000000000000000000, 1.000000000000000000 ) ) ;
#744 = CARTESIAN_POINT ( 'NONE',  ( -42.00000000000000711, 85.00000000000011369, 2.000000000000043077 ) ) ;
#745 = CARTESIAN_POINT ( 'NONE',  ( -54.99999999999990052, 7.999999999999996447, 15.49999999999877254 ) ) ;
#746 = ORIENTED_EDGE ( 'NONE', *, *, #292, .T. ) ;
#747 = ORIENTED_EDGE ( 'NONE', *, *, #7686, .F. ) ;
#748 = ORIENTED_EDGE ( 'NONE', *, *, #354, .T. ) ;
#749 = FACE_BOUND ( 'NONE', #8022, .T. ) ;
#750 = CARTESIAN_POINT ( 'NONE',  ( 41.96846535023716029, 86.62968757867487568, -1.766478104244785019 ) ) ;
#751 = DIRECTION ( 'NONE',  ( -0.000000000000000000, 1.000000000000000000, -0.000000000000000000 ) ) ;
#752 = EDGE_CURVE ( 'NONE', #6523, #4246, #5461, .T. ) ;
#753 = EDGE_CURVE ( 'NONE', #3217, #4939, #8128, .T. ) ;
#754 = EDGE_CURVE ( 'NONE', #1392, #855, #2776, .T. ) ;
#755 = AXIS2_PLACEMENT_3D ( 'NONE', #7446, #2992, #997 ) ;
#756 = CIRCLE ( 'NONE', #6069, 2.149999999999995470 ) ;
#757 = DIRECTION ( 'NONE',  ( -0.000000000000000000, -0.000000000000000000, 1.000000000000000000 ) ) ;
#758 = DIRECTION ( 'NONE',  ( -1.000000000000000000, -0.000000000000000000, -0.000000000000000000 ) ) ;
#759 = DIRECTION ( 'NONE',  ( 0.000000000000000000, 0.000000000000000000, 1.000000000000000000 ) ) ;
#760 = AXIS2_PLACEMENT_3D ( 'NONE', #3959, #712, #2125 ) ;
#761 = CARTESIAN_POINT ( 'NONE',  ( 0.000000000000000000, -1.773042676681340968, 2.059984127722458425E-15 ) ) ;
#762 = LINE ( 'NONE', #7672, #2341 ) ;
#763 = AXIS2_PLACEMENT_3D ( 'NONE', #949, #2245, #5530 ) ;
#764 = ORIENTED_EDGE ( 'NONE', *, *, #3354, .F. ) ;
#765 = DIRECTION ( 'NONE',  ( -0.000000000000000000, -0.000000000000000000, 1.000000000000000000 ) ) ;
#766 = VECTOR ( 'NONE', #3845, 1000.000000000000000 ) ;
#767 = APPLICATION_CONTEXT ( 'automotive_design' ) ;
#768 = FILL_AREA_STYLE ('',( #5810 ) ) ;
#769 = FACE_BOUND ( 'NONE', #5362, .T. ) ;
#770 = CIRCLE ( 'NONE', #7805, 3.500000000000000000 ) ;
#771 = CONICAL_SURFACE ( 'NONE', #7073, 4.000000000000000000, 1.047197551196595855 ) ;
#772 = CYLINDRICAL_SURFACE ( 'NONE', #7542, 4.999999999999993783 ) ;
#773 = AXIS2_PLACEMENT_3D ( 'NONE', #3782, #8203, #7599 ) ;
#774 = FILL_AREA_STYLE_COLOUR ( '', #7699 ) ;
#775 = VECTOR ( 'NONE', #2784, 1000.000000000000000 ) ;
#776 = EDGE_CURVE ( 'NONE', #7532, #6647, #3721, .T. ) ;
#777 = ORIENTED_EDGE ( 'NONE', *, *, #3974, .F. ) ;
#778 = CARTESIAN_POINT ( 'NONE',  ( 49.99635120648666486, 84.37668793019700786, 2.322944911472403451 ) ) ;
#779 = CIRCLE ( 'NONE', #1729, 1.280000000000000027 ) ;
#780 = ORIENTED_EDGE ( 'NONE', *, *, #5952, .F. ) ;
#781 = AXIS2_PLACEMENT_3D ( 'NONE', #7408, #5510, #7497 ) ;
#782 = ORIENTED_EDGE ( 'NONE', *, *, #6360, .T. ) ;
#783 = EDGE_LOOP ( 'NONE', ( #2328, #2669, #3779, #4427 ) ) ;
#784 = EDGE_CURVE ( 'NONE', #5142, #2405, #1146, .T. ) ;
#785 = ORIENTED_EDGE ( 'NONE', *, *, #754, .F. ) ;
#786 = CIRCLE ( 'NONE', #2249, 2.649999999999999467 ) ;
#787 = CARTESIAN_POINT ( 'NONE',  ( 60.00000000000000711, -10.00000000000000000, 60.00000000000000000 ) ) ;
#788 = CYLINDRICAL_SURFACE ( 'NONE', #7291, 4.999999999999993783 ) ;
#789 = DIRECTION ( 'NONE',  ( 1.000000000000000000, 0.000000000000000000, 0.000000000000000000 ) ) ;
#790 = CIRCLE ( 'NONE', #7560, 1.249999999999998668 ) ;
#791 = AXIS2_PLACEMENT_3D ( 'NONE', #7600, #2531, #5080 ) ;
#792 = VERTEX_POINT ( 'NONE', #4851 ) ;
#793 = ORIENTED_EDGE ( 'NONE', *, *, #60, .F. ) ;
#794 = ORIENTED_EDGE ( 'NONE', *, *, #1343, .T. ) ;
#795 = AXIS2_PLACEMENT_3D ( 'NONE', #7855, #7230, #6693 ) ;
#796 = CARTESIAN_POINT ( 'NONE',  ( -58.00000000000006395, -8.000000000000003553, 11.99999999999998934 ) ) ;
#797 = EDGE_CURVE ( 'NONE', #3149, #2513, #8163, .T. ) ;
#798 = CARTESIAN_POINT ( 'NONE',  ( 41.99105870351832692, 85.87498856589500917, -2.238438502733319790 ) ) ;
#799 = DIRECTION ( 'NONE',  ( -1.000000000000000000, -0.000000000000000000, -0.000000000000000000 ) ) ;
#800 = AXIS2_PLACEMENT_3D ( 'NONE', #6568, #4091, #5882 ) ;
#801 = EDGE_CURVE ( 'NONE', #1617, #2702, #1330, .T. ) ;
#802 =( NAMED_UNIT ( * ) SI_UNIT ( $, .STERADIAN. ) SOLID_ANGLE_UNIT ( ) );
#803 = DIRECTION ( 'NONE',  ( -1.000000000000000000, -0.000000000000000000, -0.000000000000000000 ) ) ;
#804 = CARTESIAN_POINT ( 'NONE',  ( 1.300000000000000044, -1.108512516844081475, 0.6400000000000016787 ) ) ;
#805 = CARTESIAN_POINT ( 'NONE',  ( 60.00000000000000711, 10.00000000000000000, 19.99999999999998224 ) ) ;
#806 = FACE_OUTER_BOUND ( 'NONE', #6674, .T. ) ;
#807 = CARTESIAN_POINT ( 'NONE',  ( -49.96357426530714463, 86.91018610273380318, 1.461418215542231058 ) ) ;
#808 = ORIENTED_EDGE ( 'NONE', *, *, #8120, .F. ) ;
#809 = CARTESIAN_POINT ( 'NONE',  ( -27.35000000000000497, -29.99999999999999289, 10.00000000000000000 ) ) ;
#810 = ADVANCED_FACE ( 'NONE', ( #1825 ), #1191, .T. ) ;
#811 = PLANE ( 'NONE',  #7019 ) ;
#812 = LINE ( 'NONE', #1377, #1681 ) ;
#813 = LINE ( 'NONE', #4683, #1169 ) ;
#814 = PLANE ( 'NONE',  #8086 ) ;
#815 = AXIS2_PLACEMENT_3D ( 'NONE', #7607, #3697, #7563 ) ;
#816 = CARTESIAN_POINT ( 'NONE',  ( 9.020562075079396891E-14, 10.00000000000000000, 729.2499999999977263 ) ) ;
#817 = ORIENTED_EDGE ( 'NONE', *, *, #1983, .F. ) ;
#818 = CARTESIAN_POINT ( 'NONE',  ( 49.99924596088972351, 84.68545893936931179, -2.384433782424402182 ) ) ;
#819 = UNCERTAINTY_MEASURE_WITH_UNIT (LENGTH_MEASURE( 1.000000000000000082E-05 ), #4668, 'distance_accuracy_value', 'NONE');
#820 = EDGE_CURVE ( 'NONE', #7254, #5786, #2484, .T. ) ;
#821 = VERTEX_POINT ( 'NONE', #569 ) ;
#822 = ORIENTED_EDGE ( 'NONE', *, *, #6373, .T. ) ;
#823 = CARTESIAN_POINT ( 'NONE',  ( 1.321505333908969293, -3.855830693249187480, -2.665789719053444529 ) ) ;
#824 = CARTESIAN_POINT ( 'NONE',  ( 4.200000000000001954, 2.694222958124178486E-16, 2.200000000000001066 ) ) ;
#825 = LINE ( 'NONE', #195, #3567 ) ;
#826 = ITEM_DEFINED_TRANSFORMATION ( 'NONE', 'NONE', #442,  #1587 ) ;
#827 = ORIENTED_EDGE ( 'NONE', *, *, #3693, .F. ) ;
#828 = ORIENTED_EDGE ( 'NONE', *, *, #706, .T. ) ;
#829 = ORIENTED_EDGE ( 'NONE', *, *, #2070, .F. ) ;
#830 = DIRECTION ( 'NONE',  ( 1.000000000000000000, 0.000000000000000000, 0.000000000000000000 ) ) ;
#831 = CARTESIAN_POINT ( 'NONE',  ( -3.469446951953613006E-15, 0.000000000000000000, 20.00000000000000355 ) ) ;
#832 = CARTESIAN_POINT ( 'NONE',  ( 4.200000000000001954, 0.000000000000000000, 2.000000000000000888 ) ) ;
#833 =( GEOMETRIC_REPRESENTATION_CONTEXT ( 3 ) GLOBAL_UNCERTAINTY_ASSIGNED_CONTEXT ( ( #1043 ) ) GLOBAL_UNIT_ASSIGNED_CONTEXT ( ( #7363, #5472, #1683 ) ) REPRESENTATION_CONTEXT ( 'NONE', 'WORKASPACE' ) );
#834 = PRESENTATION_STYLE_ASSIGNMENT (( #959 ) ) ;
#835 = CARTESIAN_POINT ( 'NONE',  ( 60.00000000000000711, 10.00000000000000000, 19.99999999999998224 ) ) ;
#836 = ADVANCED_FACE ( 'NONE', ( #2976 ), #4986, .T. ) ;
#837 = PRESENTATION_LAYER_ASSIGNMENT (  '', '', ( #8000 ) ) ;
#838 = EDGE_CURVE ( 'NONE', #5760, #2420, #5577, .T. ) ;
#839 = ADVANCED_FACE ( 'NONE', ( #1874 ), #6713, .F. ) ;
#840 = DIRECTION ( 'NONE',  ( 0.000000000000000000, 0.000000000000000000, -1.000000000000000000 ) ) ;
#841 = DIRECTION ( 'NONE',  ( 0.000000000000000000, 0.000000000000000000, 1.000000000000000000 ) ) ;
#842 = CYLINDRICAL_SURFACE ( 'NONE', #373, 1.249999999999998446 ) ;
#843 = AXIS2_PLACEMENT_3D ( 'NONE', #341, #6666, #5431 ) ;
#844 = FACE_OUTER_BOUND ( 'NONE', #6718, .T. ) ;
#845 = DIRECTION ( 'NONE',  ( -0.000000000000000000, -0.000000000000000000, 1.000000000000000000 ) ) ;
#846 = ORIENTED_EDGE ( 'NONE', *, *, #2319, .T. ) ;
#847 = DIRECTION ( 'NONE',  ( 0.000000000000000000, 1.000000000000000000, -0.000000000000000000 ) ) ;
#848 = DIRECTION ( 'NONE',  ( -0.000000000000000000, -0.000000000000000000, 1.000000000000000000 ) ) ;
#849 = LINE ( 'NONE', #5924, #7265 ) ;
#850 = CARTESIAN_POINT ( 'NONE',  ( 0.000000000000000000, 0.000000000000000000, -2.700000000000000178 ) ) ;
#851 = CARTESIAN_POINT ( 'NONE',  ( 1.599999999999974998, 42.68016229225776925, 4.000000000000001776 ) ) ;
#852 = ORIENTED_EDGE ( 'NONE', *, *, #1688, .T. ) ;
#853 = CARTESIAN_POINT ( 'NONE',  ( 27.34999999999998010, 30.00000000000001421, 10.00000000000000000 ) ) ;
#854 = ORIENTED_EDGE ( 'NONE', *, *, #4472, .F. ) ;
#855 = VERTEX_POINT ( 'NONE', #1019 ) ;
#856 = PLANE ( 'NONE',  #8064 ) ;
#857 = CARTESIAN_POINT ( 'NONE',  ( -27.35000000000000142, -29.99999999999999289, 4.599999999999997868 ) ) ;
#858 = DIRECTION ( 'NONE',  ( 1.000000000000000000, 0.000000000000000000, 0.000000000000000000 ) ) ;
#859 = APPLICATION_PROTOCOL_DEFINITION ( 'draft international standard', 'automotive_design', 1998, #4503 ) ;
#860 = EDGE_CURVE ( 'NONE', #6726, #3614, #3562, .T. ) ;
#861 = EDGE_LOOP ( 'NONE', ( #1217, #2447 ) ) ;
#862 = ORIENTED_EDGE ( 'NONE', *, *, #1211, .T. ) ;
#863 = VECTOR ( 'NONE', #7874, 1000.000000000000000 ) ;
#864 = ORIENTED_EDGE ( 'NONE', *, *, #4147, .T. ) ;
#865 = DIRECTION ( 'NONE',  ( 0.000000000000000000, -1.000000000000000000, 0.000000000000000000 ) ) ;
#866 = CARTESIAN_POINT ( 'NONE',  ( 29.99999999999997868, 30.00000000000001421, 10.00000000000000000 ) ) ;
#867 = DIRECTION ( 'NONE',  ( 0.000000000000000000, -0.4999999999999990563, 0.8660254037844391517 ) ) ;
#868 =( NAMED_UNIT ( * ) SI_UNIT ( $, .STERADIAN. ) SOLID_ANGLE_UNIT ( ) );
#869 = VECTOR ( 'NONE', #4101, 1000.000000000000000 ) ;
#870 = AXIS2_PLACEMENT_3D ( 'NONE', #103, #5737, #2689 ) ;
#871 = EDGE_CURVE ( 'NONE', #5289, #7139, #5484, .T. ) ;
#872 = CARTESIAN_POINT ( 'NONE',  ( 39.83716857408421674, 108.0000000000001421, 4.163336342344337027E-14 ) ) ;
#873 = DIRECTION ( 'NONE',  ( 0.000000000000000000, 0.000000000000000000, 1.000000000000000000 ) ) ;
#874 = DIRECTION ( 'NONE',  ( -1.000000000000000000, -0.000000000000000000, -0.000000000000000000 ) ) ;
#875 = B_SPLINE_CURVE_WITH_KNOTS ( 'NONE', 3,
 ( #6650, #6025, #2207, #203, #2749, #5292, #3377, #4666, #2168, #2092, #7318, #914, #2714, #5986, #247, #3500, #4704, #2797, #286, #4791, #957, #4623 ),
 .UNSPECIFIED., .F., .F.,
 ( 4, 2, 2, 2, 2, 2, 2, 2, 2, 2, 4 ),
 ( 0.01094514227676123691, 0.01231266565124741405, 0.01368018902573359119, 0.01436395071297667803, 0.01504771240021976486, 0.01641523577470593853, 0.01778275914919211220, 0.01846652083643519904, 0.01915028252367827893, 0.02051780589816445260, 0.02188532927265061934 ),
 .UNSPECIFIED. ) ;
#876 = SURFACE_SIDE_STYLE ('',( #6615 ) ) ;
#877 = ADVANCED_FACE ( 'NONE', ( #1694 ), #7995, .F. ) ;
#878 = DIRECTION ( 'NONE',  ( -1.000000000000000000, -0.000000000000000000, -0.000000000000000000 ) ) ;
#879 = CARTESIAN_POINT ( 'NONE',  ( 50.00000000000000000, -10.00000000000000000, 60.00000000000000000 ) ) ;
#880 = VECTOR ( 'NONE', #867, 1000.000000000000114 ) ;
#881 = AXIS2_PLACEMENT_3D ( 'NONE', #5603, #3643, #1102 ) ;
#882 = EDGE_LOOP ( 'NONE', ( #6137, #7790, #7495, #985 ) ) ;
#883 = CARTESIAN_POINT ( 'NONE',  ( 27.34999999999998010, 30.00000000000001421, 1.734723475976807094E-15 ) ) ;
#884 = MECHANICAL_DESIGN_GEOMETRIC_PRESENTATION_REPRESENTATION (  '', ( #8195 ), #7793 ) ;
#885 = DIRECTION ( 'NONE',  ( 0.000000000000000000, 0.000000000000000000, -1.000000000000000000 ) ) ;
#886 = ADVANCED_BREP_SHAPE_REPRESENTATION ( '', ( #1401, #1587 ), #3101 ) ;
#887 = DIRECTION ( 'NONE',  ( 0.000000000000000000, 0.000000000000000000, -1.000000000000000000 ) ) ;
#888 = CARTESIAN_POINT ( 'NONE',  ( 2.000000000000000000, 0.8865213383406723713, 1.535499999999998755 ) ) ;
#889 = DIRECTION ( 'NONE',  ( 0.000000000000000000, 1.000000000000000000, 1.224646799147353207E-16 ) ) ;
#890 = DIRECTION ( 'NONE',  ( 0.000000000000000000, 0.000000000000000000, -1.000000000000000000 ) ) ;
#891 = AXIS2_PLACEMENT_3D ( 'NONE', #5078, #7003, #1821 ) ;
#892 = CARTESIAN_POINT ( 'NONE',  ( 0.000000000000000000, 0.000000000000000000, 5.400000000000002132 ) ) ;
#893 = ORIENTED_EDGE ( 'NONE', *, *, #4371, .F. ) ;
#894 = CARTESIAN_POINT ( 'NONE',  ( 10.71950000000001424, 1.836970198721030181E-16, -1.500000000000000222 ) ) ;
#895 = EDGE_LOOP ( 'NONE', ( #149, #7973 ) ) ;
#896 = CIRCLE ( 'NONE', #3029, 1.219500000000000028 ) ;
#897 = EDGE_LOOP ( 'NONE', ( #2622, #3835 ) ) ;
#898 = AXIS2_PLACEMENT_3D ( 'NONE', #2358, #4407, #3160 ) ;
#899 = DIRECTION ( 'NONE',  ( 0.000000000000000000, 0.000000000000000000, 1.000000000000000000 ) ) ;
#900 = PRODUCT_RELATED_PRODUCT_CATEGORY ( 'part', '', ( #600 ) ) ;
#901 = AXIS2_PLACEMENT_3D ( 'NONE', #4113, #6637, #1534 ) ;
#902 = DIRECTION ( 'NONE',  ( -1.000000000000000000, 0.000000000000000000, 0.000000000000000000 ) ) ;
#903 = FACE_OUTER_BOUND ( 'NONE', #5048, .T. ) ;
#904 = EDGE_CURVE ( 'NONE', #5852, #7486, #7424, .T. ) ;
#905 = SURFACE_STYLE_FILL_AREA ( #5368 ) ;
#906 = PRODUCT_CONTEXT ( 'NONE', #2101, 'mechanical' ) ;
#907 = AXIS2_PLACEMENT_3D ( 'NONE', #7373, #1691, #936 ) ;
#908 = ORIENTED_EDGE ( 'NONE', *, *, #1318, .T. ) ;
#909 = VECTOR ( 'NONE', #6307, 1000.000000000000000 ) ;
#910 = VERTEX_POINT ( 'NONE', #6172 ) ;
#911 = EDGE_LOOP ( 'NONE', ( #160, #3033, #4699, #339 ) ) ;
#912 = TOROIDAL_SURFACE ( 'NONE', #5306, 3.299999999999999822, 0.2000000000000000111 ) ;
#913 = CYLINDRICAL_SURFACE ( 'NONE', #7698, 50.00000000000002132 ) ;
#914 = CARTESIAN_POINT ( 'NONE',  ( 5.276116561136752203, -4.623420808406671689, 8.019224293709841689 ) ) ;
#915 = AXIS2_PLACEMENT_3D ( 'NONE', #1550, #4798, #4708 ) ;
#916 = VECTOR ( 'NONE', #3282, 1000.000000000000000 ) ;
#917 = DIRECTION ( 'NONE',  ( -1.000000000000000000, 0.000000000000000000, 0.000000000000000000 ) ) ;
#918 = SHAPE_REPRESENTATION_RELATIONSHIP ( 'NONE' , 'NONE' ,  #2201, #5769 ) ;
#919 = FILL_AREA_STYLE ('',( #290 ) ) ;
#920 = EDGE_CURVE ( 'NONE', #4585, #1494, #2000, .T. ) ;
#921 = AXIS2_PLACEMENT_3D ( 'NONE', #2556, #5098, #7618 ) ;
#922 = ADVANCED_FACE ( 'NONE', ( #7467 ), #3045, .F. ) ;
#923 = CARTESIAN_POINT ( 'NONE',  ( 55.00000000000000000, 7.999999999999996447, 15.50000000000000355 ) ) ;
#924 = DIRECTION ( 'NONE',  ( -1.000000000000000000, 0.000000000000000000, 0.000000000000000000 ) ) ;
#925 = AXIS2_PLACEMENT_3D ( 'NONE', #4433, #1231, #6296 ) ;
#926 = DIRECTION ( 'NONE',  ( 0.000000000000000000, 0.000000000000000000, -1.000000000000000000 ) ) ;
#927 = APPLICATION_CONTEXT ( 'automotive_design' ) ;
#928 = AXIS2_PLACEMENT_3D ( 'NONE', #6347, #6456, #5688 ) ;
#929 = DIRECTION ( 'NONE',  ( 1.000000000000000000, 0.000000000000000000, -1.734723475976807094E-16 ) ) ;
#930 = ORIENTED_EDGE ( 'NONE', *, *, #2930, .F. ) ;
#931 = VERTEX_POINT ( 'NONE', #6838 ) ;
#932 = CARTESIAN_POINT ( 'NONE',  ( 5.000000000000015099, 4.250000000000000000, 0.000000000000000000 ) ) ;
#933 = CARTESIAN_POINT ( 'NONE',  ( 3.678949249685231848, 0.000000000000000000, -6.938893903907228378E-15 ) ) ;
#934 = CARTESIAN_POINT ( 'NONE',  ( -10.00000000000000000, 0.000000000000000000, 18.00000000000000355 ) ) ;
#935 = CARTESIAN_POINT ( 'NONE',  ( -41.93355926540179723, 87.36154593934628565, -0.4466446237679141396 ) ) ;
#936 = DIRECTION ( 'NONE',  ( 1.000000000000000000, 0.000000000000000000, 0.000000000000000000 ) ) ;
#937 = DIRECTION ( 'NONE',  ( 0.000000000000000000, 0.000000000000000000, 1.000000000000000000 ) ) ;
#938 = CARTESIAN_POINT ( 'NONE',  ( 57.99999999999999289, 7.999999999999996447, 11.99999999999998934 ) ) ;
#939 = VERTEX_POINT ( 'NONE', #5198 ) ;
#940 = LINE ( 'NONE', #5970, #5532 ) ;
#941 = EDGE_LOOP ( 'NONE', ( #412, #6401, #3522, #5747 ) ) ;
#942 = EDGE_CURVE ( 'NONE', #8148, #2793, #145, .T. ) ;
#943 = ORIENTED_EDGE ( 'NONE', *, *, #5994, .T. ) ;
#944 = CARTESIAN_POINT ( 'NONE',  ( -29.99999999999999289, 30.00000000000000711, 4.599999999999997868 ) ) ;
#945 = EDGE_CURVE ( 'NONE', #2445, #7873, #4769, .T. ) ;
#946 = CARTESIAN_POINT ( 'NONE',  ( 0.000000000000000000, 0.000000000000000000, 0.000000000000000000 ) ) ;
#947 = CARTESIAN_POINT ( 'NONE',  ( -54.99999999999990052, -8.000000000000001776, 13.34999999999877573 ) ) ;
#948 = AXIS2_PLACEMENT_3D ( 'NONE', #4184, #2277, #6673 ) ;
#949 = CARTESIAN_POINT ( 'NONE',  ( -30.00000000000000355, -29.99999999999999289, 1.734723475976807094E-15 ) ) ;
#950 = CARTESIAN_POINT ( 'NONE',  ( -2.099999999999999645, 2.571758278209440478E-16, -2.700000000000000178 ) ) ;
#951 = APPLICATION_PROTOCOL_DEFINITION ( 'draft international standard', 'automotive_design', 1998, #2101 ) ;
#952 = CIRCLE ( 'NONE', #4810, 1.535500000000000087 ) ;
#953 = VERTEX_POINT ( 'NONE', #761 ) ;
#954 = VERTEX_POINT ( 'NONE', #1916 ) ;
#955 = ORIENTED_EDGE ( 'NONE', *, *, #3106, .T. ) ;
#956 = CARTESIAN_POINT ( 'NONE',  ( 50.00000000000003553, 85.00000000000012790, 5.000000000000047073 ) ) ;
#957 = CARTESIAN_POINT ( 'NONE',  ( 7.000000000000000000, -0.4567577452614210998, 8.033969604113657681 ) ) ;
#958 = FACE_OUTER_BOUND ( 'NONE', #3987, .T. ) ;
#959 = SURFACE_STYLE_USAGE ( .BOTH. , #1639 ) ;
#960 = DIRECTION ( 'NONE',  ( -1.000000000000000000, -0.000000000000000000, -0.000000000000000000 ) ) ;
#961 = ORIENTED_EDGE ( 'NONE', *, *, #1230, .T. ) ;
#962 = LINE ( 'NONE', #4254, #7895 ) ;
#963 = ADVANCED_FACE ( 'NONE', ( #4403 ), #7637, .F. ) ;
#964 = ADVANCED_FACE ( 'NONE', ( #7715 ), #395, .F. ) ;
#965 =( GEOMETRIC_REPRESENTATION_CONTEXT ( 3 ) GLOBAL_UNCERTAINTY_ASSIGNED_CONTEXT ( ( #7136 ) ) GLOBAL_UNIT_ASSIGNED_CONTEXT ( ( #21, #2607, #1985 ) ) REPRESENTATION_CONTEXT ( 'NONE', 'WORKASPACE' ) );
#966 = DIRECTION ( 'NONE',  ( -0.000000000000000000, -0.000000000000000000, -1.000000000000000000 ) ) ;
#967 = PLANE ( 'NONE',  #3326 ) ;
#968 = EDGE_CURVE ( 'NONE', #5998, #314, #7168, .T. ) ;
#969 = CARTESIAN_POINT ( 'NONE',  ( -7.502679033599690683E-14, -4.618802153517020059, -0.3572655899081733644 ) ) ;
#970 = DIRECTION ( 'NONE',  ( -0.000000000000000000, -0.000000000000000000, 1.000000000000000000 ) ) ;
#971 = ADVANCED_FACE ( 'NONE', ( #6529 ), #2576, .T. ) ;
#972 = VERTEX_POINT ( 'NONE', #2032 ) ;
#973 = VERTEX_POINT ( 'NONE', #1405 ) ;
#974 = DIRECTION ( 'NONE',  ( -1.000000000000000000, -0.000000000000000000, -0.000000000000000000 ) ) ;
#975 = CARTESIAN_POINT ( 'NONE',  ( -7.000000000000000000, 0.000000000000000000, 18.00000000000000355 ) ) ;
#976 = AXIS2_PLACEMENT_3D ( 'NONE', #1262, #10, #3340 ) ;
#977 = CARTESIAN_POINT ( 'NONE',  ( -41.95055335361870164, 87.03835602781624914, 1.273332678597377310 ) ) ;
#978 = CARTESIAN_POINT ( 'NONE',  ( 1.300000000000000044, -1.478016689125442706, 1.843143693225357538E-15 ) ) ;
#979 = CARTESIAN_POINT ( 'NONE',  ( -49.95347202886236460, 82.84263588727921501, 1.063116165656198264 ) ) ;
#980 = LINE ( 'NONE', #938, #4549 ) ;
#981 = ORIENTED_EDGE ( 'NONE', *, *, #3877, .F. ) ;
#982 = CARTESIAN_POINT ( 'NONE',  ( -42.00000000000000711, 85.00000000000011369, -2.399999999999999911 ) ) ;
#983 = CIRCLE ( 'NONE', #3122, 2.099999999999999645 ) ;
#984 = ORIENTED_EDGE ( 'NONE', *, *, #6326, .T. ) ;
#985 = ORIENTED_EDGE ( 'NONE', *, *, #7008, .T. ) ;
#986 = CARTESIAN_POINT ( 'NONE',  ( 0.6554360035617803337, -4.240386000424090085, -2.541324518471480332 ) ) ;
#987 = DIRECTION ( 'NONE',  ( 0.000000000000000000, 0.000000000000000000, 1.000000000000000000 ) ) ;
#988 = CARTESIAN_POINT ( 'NONE',  ( 55.00000000000000000, 7.999999999999996447, 17.64999999999999858 ) ) ;
#989 = DIRECTION ( 'NONE',  ( -1.000000000000000000, 0.000000000000000000, 0.000000000000000000 ) ) ;
#990 = CARTESIAN_POINT ( 'NONE',  ( 50.00000000000000000, 10.00000000000000000, 60.00000000000000000 ) ) ;
#991 = APPLICATION_PROTOCOL_DEFINITION ( 'draft international standard', 'automotive_design', 1998, #7877 ) ;
#992 = VERTEX_POINT ( 'NONE', #3203 ) ;
#993 = ORIENTED_EDGE ( 'NONE', *, *, #5499, .F. ) ;
#994 = EDGE_LOOP ( 'NONE', ( #6655, #4917, #4187, #7876, #6236 ) ) ;
#995 = DIRECTION ( 'NONE',  ( 1.000000000000000000, 0.000000000000000000, 0.000000000000000000 ) ) ;
#996 = DIRECTION ( 'NONE',  ( 0.000000000000000000, 0.000000000000000000, -1.000000000000000000 ) ) ;
#997 = DIRECTION ( 'NONE',  ( 0.000000000000000000, 0.000000000000000000, -1.000000000000000000 ) ) ;
#998 = PRESENTATION_STYLE_ASSIGNMENT (( #5378 ) ) ;
#999 = ORIENTED_EDGE ( 'NONE', *, *, #1723, .T. ) ;
#1000 = DIRECTION ( 'NONE',  ( 0.000000000000000000, 0.000000000000000000, 1.000000000000000000 ) ) ;
#1001 = CIRCLE ( 'NONE', #4066, 1.250000000000001110 ) ;
#1002 = B_SPLINE_CURVE_WITH_KNOTS ( 'NONE', 3,
 ( #8152, #3001, #1732, #6920, #3636, #6787, #6161, #1814, #1135, #467, #5548, #4933, #6868, #557, #3677, #1180, #5638, #3772, #597, #513, #1772, #3140, #3052, #8114, #3729, #2433, #2303, #6251 ),
 .UNSPECIFIED., .F., .F.,
 ( 4, 2, 2, 2, 2, 2, 2, 2, 2, 2, 2, 2, 2, 4 ),
 ( 3.925231146709437917E-17, 0.0007633435184944741209, 0.001526687036988908994, 0.001908358796236126051, 0.002290030555483343541, 0.002671702314730560381, 0.003053374073977777655, 0.003435045833224994929, 0.003816717592472212203, 0.004198389351719429910, 0.004580061110966647184, 0.004961732870213864457, 0.005343404629461081731, 0.006106748147955515411 ),
 .UNSPECIFIED. ) ;
#1003 = CARTESIAN_POINT ( 'NONE',  ( 2.000000000000000000, 1.773042676681340968, -2.276824562219559311E-15 ) ) ;
#1004 = ADVANCED_FACE ( 'NONE', ( #4443, #3319 ), #1327, .F. ) ;
#1005 = FACE_OUTER_BOUND ( 'NONE', #340, .T. ) ;
#1006 = VECTOR ( 'NONE', #3517, 1000.000000000000000 ) ;
#1007 = CIRCLE ( 'NONE', #3821, 2.149999999999992362 ) ;
#1008 = ADVANCED_FACE ( 'NONE', ( #3156, #7748 ), #692, .F. ) ;
#1009 = EDGE_CURVE ( 'NONE', #2513, #7631, #542, .T. ) ;
#1010 = CARTESIAN_POINT ( 'NONE',  ( 2.500000000000002220, 2.357898499370434386, -3.469446951953614189E-15 ) ) ;
#1011 = FACE_OUTER_BOUND ( 'NONE', #3128, .T. ) ;
#1012 = ORIENTED_EDGE ( 'NONE', *, *, #945, .F. ) ;
#1013 = ORIENTED_EDGE ( 'NONE', *, *, #3541, .T. ) ;
#1014 = PLANE ( 'NONE',  #3687 ) ;
#1015 = CARTESIAN_POINT ( 'NONE',  ( 41.08716857408421674, 108.0000000000001421, 4.161571085597980959E-14 ) ) ;
#1016 = CARTESIAN_POINT ( 'NONE',  ( -41.97904239022133055, 86.32664991614245764, 2.000000000000043521 ) ) ;
#1017 = CARTESIAN_POINT ( 'NONE',  ( 1.300000000000000044, 1.478016689125442484, -1.626303258728256651E-15 ) ) ;
#1018 = LINE ( 'NONE', #5356, #7945 ) ;
#1019 = CARTESIAN_POINT ( 'NONE',  ( 2.500000000000000444, 0.000000000000000000, 3.469446951953614189E-15 ) ) ;
#1020 = ORIENTED_EDGE ( 'NONE', *, *, #4149, .F. ) ;
#1021 = DIRECTION ( 'NONE',  ( 1.000000000000000000, 0.000000000000000000, 0.000000000000000000 ) ) ;
#1022 = ORIENTED_EDGE ( 'NONE', *, *, #3595, .F. ) ;
#1023 = ORIENTED_EDGE ( 'NONE', *, *, #4321, .F. ) ;
#1024 = CIRCLE ( 'NONE', #636, 2.000000000000000444 ) ;
#1025 = CARTESIAN_POINT ( 'NONE',  ( 5.200000000000020606, 0.000000000000000000, -6.938893903907228378E-15 ) ) ;
#1026 = DIRECTION ( 'NONE',  ( 0.000000000000000000, 0.000000000000000000, 1.000000000000000000 ) ) ;
#1027 = DIRECTION ( 'NONE',  ( 1.000000000000000000, 0.000000000000000000, 0.000000000000000000 ) ) ;
#1028 = EDGE_CURVE ( 'NONE', #7060, #5289, #1883, .T. ) ;
#1029 = FACE_OUTER_BOUND ( 'NONE', #1141, .T. ) ;
#1030 = LINE ( 'NONE', #990, #5691 ) ;
#1031 = CONTEXT_DEPENDENT_SHAPE_REPRESENTATION ( #3925, #530 ) ;
#1032 = AXIS2_PLACEMENT_3D ( 'NONE', #745, #2051, #5285 ) ;
#1033 = CONICAL_SURFACE ( 'NONE', #2227, 4.000000000000000000, 1.047197551196595855 ) ;
#1034 = ADVANCED_FACE ( 'NONE', ( #655 ), #5850, .F. ) ;
#1035 = AXIS2_PLACEMENT_3D ( 'NONE', #6976, #1250, #5657 ) ;
#1036 = EDGE_LOOP ( 'NONE', ( #4205, #862, #2315, #3701 ) ) ;
#1037 = VERTEX_POINT ( 'NONE', #3239 ) ;
#1038 = VERTEX_POINT ( 'NONE', #1283 ) ;
#1039 = CARTESIAN_POINT ( 'NONE',  ( 0.000000000000000000, 0.000000000000000000, 0.000000000000000000 ) ) ;
#1040 = CARTESIAN_POINT ( 'NONE',  ( 2.000000000000000000, 1.773042676681340968, -2.276824562219559311E-15 ) ) ;
#1041 = CARTESIAN_POINT ( 'NONE',  ( -25.00000000000000711, -29.99999999999999289, 4.599999999999997868 ) ) ;
#1042 = AXIS2_PLACEMENT_3D ( 'NONE', #8002, #5404, #6140 ) ;
#1043 = UNCERTAINTY_MEASURE_WITH_UNIT (LENGTH_MEASURE( 1.000000000000000082E-05 ), #7363, 'distance_accuracy_value', 'NONE');
#1044 = AXIS2_PLACEMENT_3D ( 'NONE', #5735, #7005, #1323 ) ;
#1045 = VECTOR ( 'NONE', #4892, 1000.000000000000000 ) ;
#1046 = ORIENTED_EDGE ( 'NONE', *, *, #7455, .T. ) ;
#1047 = CARTESIAN_POINT ( 'NONE',  ( 4.000000000000002665, 1.935983797701077869, -0.2494693066162346762 ) ) ;
#1048 = ORIENTED_EDGE ( 'NONE', *, *, #8164, .F. ) ;
#1049 = VECTOR ( 'NONE', #4012, 1000.000000000000000 ) ;
#1050 = ADVANCED_FACE ( 'NONE', ( #3273 ), #5771, .F. ) ;
#1051 = AXIS2_PLACEMENT_3D ( 'NONE', #2804, #3507, #5344 ) ;
#1052 = CARTESIAN_POINT ( 'NONE',  ( -39.99999999999999289, -39.99999999999999289, 10.00000000000000000 ) ) ;
#1053 = ADVANCED_FACE ( 'NONE', ( #1996 ), #7051, .F. ) ;
#1054 = DIRECTION ( 'NONE',  ( 1.000000000000000000, 0.000000000000000000, 0.000000000000000000 ) ) ;
#1055 = PRODUCT_DEFINITION_SHAPE ( 'NONE', 'NONE',  #1782 ) ;
#1056 = DIRECTION ( 'NONE',  ( 1.412205397084881070E-17, -2.775557561562891967E-17, -1.000000000000000000 ) ) ;
#1057 = FACE_OUTER_BOUND ( 'NONE', #7251, .T. ) ;
#1058 = EDGE_CURVE ( 'NONE', #6819, #2818, #1552, .T. ) ;
#1059 = ORIENTED_EDGE ( 'NONE', *, *, #7565, .F. ) ;
#1060 = COLOUR_RGB ( '', 0.40784314, 0.44705882, 0.49803922) ;
#1061 = ORIENTED_EDGE ( 'NONE', *, *, #2412, .T. ) ;
#1062 = CARTESIAN_POINT ( 'NONE',  ( 2.000000000000000000, -1.773042676681340968, 2.059984127722458425E-15 ) ) ;
#1063 = CARTESIAN_POINT ( 'NONE',  ( -2.678494666091066012, -3.072372537026387018, -0.03421028094655010482 ) ) ;
#1064 = DIRECTION ( 'NONE',  ( 1.000000000000000000, 0.000000000000000000, 0.000000000000000000 ) ) ;
#1065 = CARTESIAN_POINT ( 'NONE',  ( -49.98566918070725507, 83.79593159430156390, -2.081985610399898157 ) ) ;
#1066 = COLOUR_RGB ( '', 0.09019608, 0.27058824, 0.51372549) ;
#1067 = DIRECTION ( 'NONE',  ( 0.000000000000000000, 1.224646799147353207E-16, 1.000000000000000000 ) ) ;
#1068 = EDGE_LOOP ( 'NONE', ( #6038, #2674, #6851, #8178 ) ) ;
#1069 = DIRECTION ( 'NONE',  ( 0.000000000000000000, 0.000000000000000000, -1.000000000000000000 ) ) ;
#1070 = ADVANCED_FACE ( 'NONE', ( #4597, #7827, #3384, #5307, #2141 ), #6617, .F. ) ;
#1071 = ORIENTED_EDGE ( 'NONE', *, *, #8119, .F. ) ;
#1072 = EDGE_CURVE ( 'NONE', #5459, #8175, #5974, .T. ) ;
#1073 = EDGE_LOOP ( 'NONE', ( #6447, #5983, #2589, #4040 ) ) ;
#1074 = CARTESIAN_POINT ( 'NONE',  ( 41.97904239022138029, 86.32664991614251448, 2.000000000000043521 ) ) ;
#1075 = CARTESIAN_POINT ( 'NONE',  ( -7.502679033599690683E-14, -4.618802153517020059, -0.3572655899081733644 ) ) ;
#1076 = DIRECTION ( 'NONE',  ( -1.000000000000000000, 0.000000000000000000, 1.032573497605241731E-17 ) ) ;
#1077 = FACE_OUTER_BOUND ( 'NONE', #695, .T. ) ;
#1078 = FACE_OUTER_BOUND ( 'NONE', #5758, .T. ) ;
#1079 = ADVANCED_FACE ( 'NONE', ( #4676, #2844 ), #4131, .T. ) ;
#1080 = ORIENTED_EDGE ( 'NONE', *, *, #6298, .T. ) ;
#1081 = VERTEX_POINT ( 'NONE', #7286 ) ;
#1082 = ORIENTED_EDGE ( 'NONE', *, *, #4413, .T. ) ;
#1083 = CARTESIAN_POINT ( 'NONE',  ( -60.00000000000000000, -10.00000000000000000, 10.50000000000000000 ) ) ;
#1084 = DIRECTION ( 'NONE',  ( -1.000000000000000000, -0.000000000000000000, -0.000000000000000000 ) ) ;
#1085 = DIRECTION ( 'NONE',  ( 1.000000000000000000, 0.000000000000000000, 0.000000000000000000 ) ) ;
#1086 = CIRCLE ( 'NONE', #559, 42.00000000000002132 ) ;
#1087 = ORIENTED_EDGE ( 'NONE', *, *, #5273, .F. ) ;
#1088 = DIRECTION ( 'NONE',  ( -1.000000000000000000, 0.000000000000000000, 0.000000000000000000 ) ) ;
#1089 = ORIENTED_EDGE ( 'NONE', *, *, #551, .T. ) ;
#1090 = ORIENTED_EDGE ( 'NONE', *, *, #4303, .F. ) ;
#1091 = DIRECTION ( 'NONE',  ( -0.000000000000000000, 1.000000000000000000, -0.000000000000000000 ) ) ;
#1092 = DIRECTION ( 'NONE',  ( 1.000000000000000000, -0.000000000000000000, -0.000000000000000000 ) ) ;
#1093 = FILL_AREA_STYLE_COLOUR ( '', #7081 ) ;
#1094 = CYLINDRICAL_SURFACE ( 'NONE', #4649, 1.250000000000001110 ) ;
#1095 = ADVANCED_FACE ( 'NONE', ( #806 ), #7897, .T. ) ;
#1096 = DIRECTION ( 'NONE',  ( 0.000000000000000000, 0.000000000000000000, 1.000000000000000000 ) ) ;
#1097 = EDGE_CURVE ( 'NONE', #6822, #157, #3510, .T. ) ;
#1098 = ADVANCED_FACE ( 'NONE', ( #844 ), #7167, .F. ) ;
#1099 = PRODUCT_DEFINITION_FORMATION_WITH_SPECIFIED_SOURCE ( 'ANY', '', #5068, .NOT_KNOWN. ) ;
#1100 = ORIENTED_EDGE ( 'NONE', *, *, #1276, .T. ) ;
#1101 = EDGE_LOOP ( 'NONE', ( #4231, #1354, #3513, #6258 ) ) ;
#1102 = DIRECTION ( 'NONE',  ( -1.000000000000000000, 0.000000000000000000, 0.000000000000000000 ) ) ;
#1103 = CARTESIAN_POINT ( 'NONE',  ( -42.00000000000001421, 85.25445652427316645, -2.400000000000036326 ) ) ;
#1104 = DIRECTION ( 'NONE',  ( 1.000000000000000000, 0.000000000000000000, 0.000000000000000000 ) ) ;
#1105 = LINE ( 'NONE', #1196, #6872 ) ;
#1106 = STYLED_ITEM ( 'NONE', ( #5550 ), #293 ) ;
#1107 = DIRECTION ( 'NONE',  ( 0.000000000000000000, 1.000000000000000000, -0.000000000000000000 ) ) ;
#1108 = DIRECTION ( 'NONE',  ( 0.000000000000000000, 0.000000000000000000, -1.000000000000000000 ) ) ;
#1109 = ORIENTED_EDGE ( 'NONE', *, *, #3372, .T. ) ;
#1110 = VERTEX_POINT ( 'NONE', #1606 ) ;
#1111 = AXIS2_PLACEMENT_3D ( 'NONE', #5867, #129, #3885 ) ;
#1112 = FACE_OUTER_BOUND ( 'NONE', #3633, .T. ) ;
#1113 = LINE ( 'NONE', #7561, #7414 ) ;
#1114 = FACE_BOUND ( 'NONE', #3753, .T. ) ;
#1115 = CARTESIAN_POINT ( 'NONE',  ( -4.000000000000000000, -1.933795701539609668, -0.2488376576622978453 ) ) ;
#1116 = CARTESIAN_POINT ( 'NONE',  ( -1.809537700406288696, 6.765955536481263799, 8.002236580937831079 ) ) ;
#1117 = EDGE_CURVE ( 'NONE', #2702, #6185, #2402, .T. ) ;
#1118 = LINE ( 'NONE', #539, #4085 ) ;
#1119 = VECTOR ( 'NONE', #2487, 1000.000000000000114 ) ;
#1120 = EDGE_LOOP ( 'NONE', ( #2459, #4178 ) ) ;
#1121 = ORIENTED_EDGE ( 'NONE', *, *, #3316, .F. ) ;
#1122 = EDGE_LOOP ( 'NONE', ( #573, #785 ) ) ;
#1123 = EDGE_LOOP ( 'NONE', ( #6954, #2857 ) ) ;
#1124 = PRODUCT_DEFINITION_SHAPE ( 'NONE', 'NONE',  #7899 ) ;
#1125 = DIRECTION ( 'NONE',  ( -1.000000000000000000, 0.000000000000000000, 1.412205397084881070E-17 ) ) ;
#1126 = CARTESIAN_POINT ( 'NONE',  ( 0.2500000000000002220, 0.000000000000000000, 2.081668171172168513E-14 ) ) ;
#1127 = LINE ( 'NONE', #6150, #6601 ) ;
#1128 = EDGE_CURVE ( 'NONE', #6469, #3165, #5928, .T. ) ;
#1129 =( NAMED_UNIT ( * ) SI_UNIT ( $, .STERADIAN. ) SOLID_ANGLE_UNIT ( ) );
#1130 = EDGE_LOOP ( 'NONE', ( #3957, #6831, #3928, #2663 ) ) ;
#1131 = CYLINDRICAL_SURFACE ( 'NONE', #4595, 4.999999999999993783 ) ;
#1132 = VERTEX_POINT ( 'NONE', #2100 ) ;
#1133 = ORIENTED_EDGE ( 'NONE', *, *, #5507, .T. ) ;
#1134 = CARTESIAN_POINT ( 'NONE',  ( -1.599999999999986766, 37.49999999999999289, 4.000000000000001776 ) ) ;
#1135 = CARTESIAN_POINT ( 'NONE',  ( -41.93161960896017604, 82.60431869815872119, 0.1926422142525844872 ) ) ;
#1137 = EDGE_CURVE ( 'NONE', #4618, #3296, #6387, .T. ) ;
#1136 =( NAMED_UNIT ( * ) SI_UNIT ( $, .STERADIAN. ) SOLID_ANGLE_UNIT ( ) );
#1138 = FILL_AREA_STYLE_COLOUR ( '', #1066 ) ;
#1139 = CARTESIAN_POINT ( 'NONE',  ( 2.500000000000002220, 2.357898499370434386, -3.469446951953614189E-15 ) ) ;
#1140 = ORIENTED_EDGE ( 'NONE', *, *, #7176, .T. ) ;
#1141 = EDGE_LOOP ( 'NONE', ( #7138, #4109, #4365, #6940, #3679 ) ) ;
#1142 = CONICAL_SURFACE ( 'NONE', #3816, 1.610000000000000098, 0.7853981633974652654 ) ;
#1143 = DIRECTION ( 'NONE',  ( 1.000000000000000000, 1.502586498047605218E-16, -1.412205397084881070E-17 ) ) ;
#1144 = DIRECTION ( 'NONE',  ( -1.000000000000000000, 0.000000000000000000, 1.412205397084726379E-17 ) ) ;
#1145 = CARTESIAN_POINT ( 'NONE',  ( 0.1499999999999973577, 0.000000000000000000, 2.750000000000000000 ) ) ;
#1146 = LINE ( 'NONE', #3686, #2655 ) ;
#1147 = ORIENTED_EDGE ( 'NONE', *, *, #5934, .F. ) ;
#1148 = ORIENTED_EDGE ( 'NONE', *, *, #6993, .T. ) ;
#1149 = CARTESIAN_POINT ( 'NONE',  ( -4.000000000000000000, 0.3904826640788065517, -2.700000000000001510 ) ) ;
#1150 = DIRECTION ( 'NONE',  ( -1.000000000000000000, 0.000000000000000000, -0.000000000000000000 ) ) ;
#1151 = CARTESIAN_POINT ( 'NONE',  ( -2.099999999999999645, 2.571758278209440478E-16, -2.394516984716111185 ) ) ;
#1152 = PLANE ( 'NONE',  #2816 ) ;
#1153 = PLANE ( 'NONE',  #1035 ) ;
#1154 = LINE ( 'NONE', #4956, #4353 ) ;
#1155 = ITEM_DEFINED_TRANSFORMATION ( 'NONE', 'NONE', #4567,  #1587 ) ;
#1156 = VERTEX_POINT ( 'NONE', #336 ) ;
#1157 = VECTOR ( 'NONE', #917, 1000.000000000000000 ) ;
#1158 = VERTEX_POINT ( 'NONE', #5957 ) ;
#1159 = EDGE_CURVE ( 'NONE', #3778, #604, #1443, .T. ) ;
#1160 = AXIS2_PLACEMENT_3D ( 'NONE', #6041, #2890, #5432 ) ;
#1161 = ORIENTED_EDGE ( 'NONE', *, *, #6259, .T. ) ;
#1162 = ORIENTED_EDGE ( 'NONE', *, *, #6234, .T. ) ;
#1163 = ADVANCED_FACE ( 'NONE', ( #2760 ), #2066, .T. ) ;
#1164 = CARTESIAN_POINT ( 'NONE',  ( 1.250000000000003997, 38.99999999999999289, 1.765256746356098409E-17 ) ) ;
#1165 = AXIS2_PLACEMENT_3D ( 'NONE', #3394, #6464, #1339 ) ;
#1166 = DIRECTION ( 'NONE',  ( 0.000000000000000000, -0.000000000000000000, -1.000000000000000000 ) ) ;
#1167 = CARTESIAN_POINT ( 'NONE',  ( 27.35000000000001208, -29.99999999999997868, 4.599999999999997868 ) ) ;
#1168 = FILL_AREA_STYLE ('',( #6910 ) ) ;
#1169 = VECTOR ( 'NONE', #6434, 1000.000000000000000 ) ;
#1170 = AXIS2_PLACEMENT_3D ( 'NONE', #3288, #7106, #278 ) ;
#1171 = VERTEX_POINT ( 'NONE', #178 ) ;
#1172 = CARTESIAN_POINT ( 'NONE',  ( 49.94600989915087297, 82.67684773840547052, 0.6225708050466158827 ) ) ;
#1173 = ORIENTED_EDGE ( 'NONE', *, *, #5153, .T. ) ;
#1174 = ORIENTED_EDGE ( 'NONE', *, *, #1998, .F. ) ;
#1175 = CIRCLE ( 'NONE', #5826, 2.649999999999995026 ) ;
#1176 = CIRCLE ( 'NONE', #1042, 2.000000000000000444 ) ;
#1177 = AXIS2_PLACEMENT_3D ( 'NONE', #2685, #7712, #2029 ) ;
#1179 = DIRECTION ( 'NONE',  ( 1.000000000000000000, 0.000000000000000000, 0.000000000000000000 ) ) ;
#1178 = AXIS2_PLACEMENT_3D ( 'NONE', #3683, #6835, #2439 ) ;
#1180 = CARTESIAN_POINT ( 'NONE',  ( -41.94739886896328329, 82.89789273483425802, -1.165086683815163449 ) ) ;
#1181 = CARTESIAN_POINT ( 'NONE',  ( 0.000000000000000000, 37.49999999999999289, 4.000000000000001776 ) ) ;
#1182 = VECTOR ( 'NONE', #8132, 1000.000000000000000 ) ;
#1183 =( LENGTH_UNIT ( ) NAMED_UNIT ( * ) SI_UNIT ( .MILLI., .METRE. ) );
#1184 = EDGE_CURVE ( 'NONE', #4714, #5524, #2806, .T. ) ;
#1185 = PLANE ( 'NONE',  #6273 ) ;
#1186 = AXIS2_PLACEMENT_3D ( 'NONE', #2421, #6065, #4328 ) ;
#1187 = PRESENTATION_LAYER_ASSIGNMENT (  '', '', ( #2652 ) ) ;
#1188 =( REPRESENTATION_RELATIONSHIP ('NONE','NONE', #3916, #7870 ) REPRESENTATION_RELATIONSHIP_WITH_TRANSFORMATION ( #6896 )SHAPE_REPRESENTATION_RELATIONSHIP( ) );
#1189 = EDGE_LOOP ( 'NONE', ( #4336, #622, #5682, #3680 ) ) ;
#1190 = ORIENTED_EDGE ( 'NONE', *, *, #7346, .T. ) ;
#1191 = CONICAL_SURFACE ( 'NONE', #5709, 4.000000000000000000, 1.047197551196595855 ) ;
#1192 = CARTESIAN_POINT ( 'NONE',  ( 3.000000000000000888, 0.000000000000000000, 0.000000000000000000 ) ) ;
#1193 = AXIS2_PLACEMENT_3D ( 'NONE', #1933, #5753, #5667 ) ;
#1194 = DIRECTION ( 'NONE',  ( -0.000000000000000000, -1.000000000000000000, -0.000000000000000000 ) ) ;
#1195 = PLANE ( 'NONE',  #773 ) ;
#1196 = CARTESIAN_POINT ( 'NONE',  ( 42.00000000000003553, 85.00000000000012790, 5.000000000000045297 ) ) ;
#1197 = VECTOR ( 'NONE', #3237, 1000.000000000000000 ) ;
#1198 = AXIS2_PLACEMENT_3D ( 'NONE', #6345, #1824, #3155 ) ;
#1199 = DIRECTION ( 'NONE',  ( 0.000000000000000000, 0.000000000000000000, -1.000000000000000000 ) ) ;
#1200 = LINE ( 'NONE', #6929, #6572 ) ;
#1201 = PRODUCT ( 'H_bar', 'H_bar', '', ( #3408 ) ) ;
#1202 = VECTOR ( 'NONE', #1084, 1000.000000000000000 ) ;
#1203 = ORIENTED_EDGE ( 'NONE', *, *, #2986, .F. ) ;
#1204 = CARTESIAN_POINT ( 'NONE',  ( 20.00000000000000000, 1.610000000000000098, 0.000000000000000000 ) ) ;
#1205 = CARTESIAN_POINT ( 'NONE',  ( 55.00000000000000000, -8.000000000000001776, 13.35000000000000853 ) ) ;
#1206 = DIRECTION ( 'NONE',  ( -0.000000000000000000, 0.000000000000000000, 1.000000000000000000 ) ) ;
#1207 = DIRECTION ( 'NONE',  ( 0.000000000000000000, 0.000000000000000000, 1.000000000000000000 ) ) ;
#1208 = CARTESIAN_POINT ( 'NONE',  ( 2.500000000000002220, 2.357898499370434386, -3.469446951953614189E-15 ) ) ;
#1209 = LINE ( 'NONE', #37, #3965 ) ;
#1210 = ORIENTED_EDGE ( 'NONE', *, *, #4128, .T. ) ;
#1211 = EDGE_CURVE ( 'NONE', #2407, #6822, #7828, .T. ) ;
#1212 = EDGE_CURVE ( 'NONE', #6705, #244, #6254, .T. ) ;
#1213 = EDGE_LOOP ( 'NONE', ( #6439, #7962 ) ) ;
#1214 = ADVANCED_FACE ( 'NONE', ( #4883 ), #4003, .T. ) ;
#1215 = DIRECTION ( 'NONE',  ( 0.000000000000000000, 0.4999999999999990008, -0.8660254037844391517 ) ) ;
#1216 = VERTEX_POINT ( 'NONE', #2928 ) ;
#1217 = ORIENTED_EDGE ( 'NONE', *, *, #2136, .T. ) ;
#1218 = CARTESIAN_POINT ( 'NONE',  ( 1.300000000000000044, 1.478016689125442484, -1.626303258728256651E-15 ) ) ;
#1219 = DIRECTION ( 'NONE',  ( -0.000000000000000000, -0.000000000000000000, 1.000000000000000000 ) ) ;
#1220 = DIRECTION ( 'NONE',  ( -0.000000000000000000, -0.000000000000000000, 1.000000000000000000 ) ) ;
#1221 = EDGE_LOOP ( 'NONE', ( #5440, #1947 ) ) ;
#1222 = CARTESIAN_POINT ( 'NONE',  ( 49.94236411077207549, 82.59994436935576800, 0.1557065084606094330 ) ) ;
#1223 = EDGE_LOOP ( 'NONE', ( #7509, #3451, #6070, #8010 ) ) ;
#1224 = ORIENTED_EDGE ( 'NONE', *, *, #6422, .F. ) ;
#1225 = CARTESIAN_POINT ( 'NONE',  ( 2.000000000000000000, -0.8865213383406685965, 1.535500000000000531 ) ) ;
#1226 = DIRECTION ( 'NONE',  ( 1.000000000000000000, 0.000000000000000000, 0.000000000000000000 ) ) ;
#1227 = FACE_OUTER_BOUND ( 'NONE', #4610, .T. ) ;
#1228 = AXIS2_PLACEMENT_3D ( 'NONE', #4153, #3575, #6588 ) ;
#1229 = FILL_AREA_STYLE ('',( #1093 ) ) ;
#1230 = EDGE_CURVE ( 'NONE', #1132, #3745, #6871, .T. ) ;
#1231 = DIRECTION ( 'NONE',  ( 1.000000000000000000, -0.000000000000000000, -0.000000000000000000 ) ) ;
#1232 = DIRECTION ( 'NONE',  ( 0.000000000000000000, -0.4999999999999991118, 0.8660254037844391517 ) ) ;
#1233 = CIRCLE ( 'NONE', #7066, 1.500000000000000222 ) ;
#1234 = ORIENTED_EDGE ( 'NONE', *, *, #4481, .F. ) ;
#1235 = VERTEX_POINT ( 'NONE', #5473 ) ;
#1236 = ADVANCED_FACE ( 'NONE', ( #2392 ), #3003, .F. ) ;
#1237 = DIRECTION ( 'NONE',  ( -1.000000000000000000, -0.000000000000000000, -0.000000000000000000 ) ) ;
#1238 = DIRECTION ( 'NONE',  ( 0.000000000000000000, 0.4999999999999991673, -0.8660254037844391517 ) ) ;
#1239 = CYLINDRICAL_SURFACE ( 'NONE', #1995, 4.999999999999997335 ) ;
#1240 = LINE ( 'NONE', #6306, #3589 ) ;
#1241 = EDGE_CURVE ( 'NONE', #531, #3462, #11, .T. ) ;
#1242 = CARTESIAN_POINT ( 'NONE',  ( -54.99999999999990052, -8.000000000000001776, 15.49999999999877254 ) ) ;
#1243 = DIRECTION ( 'NONE',  ( 1.000000000000000000, 0.000000000000000000, 0.000000000000000000 ) ) ;
#1244 = ORIENTED_EDGE ( 'NONE', *, *, #2547, .T. ) ;
#1245 = FACE_BOUND ( 'NONE', #1120, .T. ) ;
#1246 = CARTESIAN_POINT ( 'NONE',  ( 2.886521338340684917, 0.000000000000000000, 0.000000000000000000 ) ) ;
#1247 = MANIFOLD_SOLID_BREP ( 'Hex', #5947 ) ;
#1248 = DIRECTION ( 'NONE',  ( 0.000000000000000000, 1.000000000000000000, -0.000000000000000000 ) ) ;
#1249 =( GEOMETRIC_REPRESENTATION_CONTEXT ( 3 ) GLOBAL_UNCERTAINTY_ASSIGNED_CONTEXT ( ( #6118 ) ) GLOBAL_UNIT_ASSIGNED_CONTEXT ( ( #1271, #6870, #1733 ) ) REPRESENTATION_CONTEXT ( 'NONE', 'WORKASPACE' ) );
#1250 = DIRECTION ( 'NONE',  ( 0.000000000000000000, -1.222984857324291014E-15, -1.000000000000000000 ) ) ;
#1251 = CARTESIAN_POINT ( 'NONE',  ( 49.96366046868875088, 86.90794461356699685, 1.464368789227024736 ) ) ;
#1252 = EDGE_LOOP ( 'NONE', ( #4195, #5505 ) ) ;
#1253 = MECHANICAL_DESIGN_GEOMETRIC_PRESENTATION_REPRESENTATION (  '', ( #7490 ), #5889 ) ;
#1254 = ORIENTED_EDGE ( 'NONE', *, *, #3053, .F. ) ;
#1255 = CARTESIAN_POINT ( 'NONE',  ( -3.000000000000000888, 45.09008114612887397, 0.000000000000000000 ) ) ;
#1256 = PRODUCT_DEFINITION_CONTEXT ( 'detailed design', #509, 'design' ) ;
#1257 = EDGE_LOOP ( 'NONE', ( #5536, #2886 ) ) ;
#1258 = VERTEX_POINT ( 'NONE', #4935 ) ;
#1259 = CARTESIAN_POINT ( 'NONE',  ( -41.99795150464620974, 84.52878598459807336, 2.364843771231078584 ) ) ;
#1260 = DIRECTION ( 'NONE',  ( 0.000000000000000000, 0.000000000000000000, 1.000000000000000000 ) ) ;
#1261 = DIRECTION ( 'NONE',  ( -1.000000000000000000, -0.000000000000000000, -0.000000000000000000 ) ) ;
#1262 = CARTESIAN_POINT ( 'NONE',  ( -39.83716857408442991, 124.0119620251977040, 12.00000000000001421 ) ) ;
#1263 = VERTEX_POINT ( 'NONE', #4263 ) ;
#1264 = CARTESIAN_POINT ( 'NONE',  ( 49.94237215279112263, 82.60011171831010302, -0.3139783802612605146 ) ) ;
#1265 = ORIENTED_EDGE ( 'NONE', *, *, #1900, .F. ) ;
#1266 = ORIENTED_EDGE ( 'NONE', *, *, #1957, .F. ) ;
#1267 = LINE ( 'NONE', #7624, #4912 ) ;
#1268 = CARTESIAN_POINT ( 'NONE',  ( 41.97224931050730845, 83.45839738397258145, 1.857416509361046630 ) ) ;
#1269 = DIRECTION ( 'NONE',  ( 0.000000000000000000, 0.000000000000000000, 1.000000000000000000 ) ) ;
#1270 = ADVANCED_FACE ( 'NONE', ( #1773 ), #1094, .F. ) ;
#1271 =( LENGTH_UNIT ( ) NAMED_UNIT ( * ) SI_UNIT ( .MILLI., .METRE. ) );
#1272 = PRODUCT_DEFINITION_SHAPE ( 'NONE', 'NONE',  #8212 ) ;
#1273 = FACE_OUTER_BOUND ( 'NONE', #5568, .T. ) ;
#1274 = EDGE_CURVE ( 'NONE', #2969, #7545, #6079, .T. ) ;
#1275 = ORIENTED_EDGE ( 'NONE', *, *, #838, .F. ) ;
#1276 = EDGE_CURVE ( 'NONE', #4446, #7545, #2128, .T. ) ;
#1277 = EDGE_CURVE ( 'NONE', #5489, #8148, #8025, .T. ) ;
#1278 = LINE ( 'NONE', #1439, #3861 ) ;
#1279 = CARTESIAN_POINT ( 'NONE',  ( 0.000000000000000000, 0.000000000000000000, 0.000000000000000000 ) ) ;
#1280 = CARTESIAN_POINT ( 'NONE',  ( -60.00000000000000000, -10.00000000000000000, 20.00000000000000355 ) ) ;
#1281 = DIRECTION ( 'NONE',  ( 0.000000000000000000, 0.000000000000000000, 1.000000000000000000 ) ) ;
#1282 = EDGE_CURVE ( 'NONE', #5386, #4369, #4820, .T. ) ;
#1283 = CARTESIAN_POINT ( 'NONE',  ( 27.35000000000001208, -29.99999999999997868, 1.734723475976807094E-15 ) ) ;
#1284 = CARTESIAN_POINT ( 'NONE',  ( -49.99683717277851258, 85.63216245974585661, 2.336254100262071809 ) ) ;
#1285 = AXIS2_PLACEMENT_3D ( 'NONE', #6028, #4968, #375 ) ;
#1286 = ORIENTED_EDGE ( 'NONE', *, *, #5596, .T. ) ;
#1287 = LINE ( 'NONE', #5085, #2062 ) ;
#1288 = LINE ( 'NONE', #662, #7146 ) ;
#1289 = DIRECTION ( 'NONE',  ( 0.000000000000000000, 0.000000000000000000, -1.000000000000000000 ) ) ;
#1290 = DIRECTION ( 'NONE',  ( -0.000000000000000000, -0.000000000000000000, 1.000000000000000000 ) ) ;
#1291 = CARTESIAN_POINT ( 'NONE',  ( 0.000000000000000000, 1.773042676681340968, -2.276824562219559311E-15 ) ) ;
#1292 = TOROIDAL_SURFACE ( 'NONE', #2340, 3.299999999999999822, 0.2000000000000000111 ) ;
#1293 = AXIS2_PLACEMENT_3D ( 'NONE', #30, #4562, #1917 ) ;
#1294 = ORIENTED_EDGE ( 'NONE', *, *, #1938, .F. ) ;
#1295 = EDGE_LOOP ( 'NONE', ( #7925, #7105 ) ) ;
#1296 = CARTESIAN_POINT ( 'NONE',  ( 41.99057456900149532, 84.08235334355106261, 2.230005891995792133 ) ) ;
#1297 = VERTEX_POINT ( 'NONE', #7663 ) ;
#1298 = EDGE_CURVE ( 'NONE', #3935, #7038, #4529, .T. ) ;
#1299 = ORIENTED_EDGE ( 'NONE', *, *, #6393, .T. ) ;
#1300 = CARTESIAN_POINT ( 'NONE',  ( 1.599999999999998979, 37.49999999999999289, 0.000000000000000000 ) ) ;
#1301 = FACE_OUTER_BOUND ( 'NONE', #5738, .T. ) ;
#1302 = DIRECTION ( 'NONE',  ( 0.000000000000000000, 0.000000000000000000, 1.000000000000000000 ) ) ;
#1303 = CARTESIAN_POINT ( 'NONE',  ( 110.0000000000000995, 46.01196202519845713, -3.266478619163291162E-15 ) ) ;
#1304 = VECTOR ( 'NONE', #5066, 1000.000000000000000 ) ;
#1305 = ORIENTED_EDGE ( 'NONE', *, *, #6099, .F. ) ;
#1306 = AXIS2_PLACEMENT_3D ( 'NONE', #2270, #5477, #7989 ) ;
#1307 = ORIENTED_EDGE ( 'NONE', *, *, #1889, .T. ) ;
#1308 = ORIENTED_EDGE ( 'NONE', *, *, #400, .T. ) ;
#1309 = LINE ( 'NONE', #5835, #1866 ) ;
#1310 = CARTESIAN_POINT ( 'NONE',  ( 41.93910753963084659, 87.26111082761428861, -0.8146863085835460705 ) ) ;
#1311 = CARTESIAN_POINT ( 'NONE',  ( 2.000000000000000000, -0.8865213383406685965, 1.535500000000000531 ) ) ;
#1312 = AXIS2_PLACEMENT_3D ( 'NONE', #4807, #4847, #7334 ) ;
#1313 = CARTESIAN_POINT ( 'NONE',  ( -0.4566803630309465567, -7.000000000000006217, 8.000000000000042633 ) ) ;
#1314 = SHAPE_REPRESENTATION ( 'hex thin nut chamfered gradeab_iso_ISO - 4035 - M5 - N', ( #1587 ), #2305 ) ;
#1315 = ADVANCED_FACE ( 'NONE', ( #4557 ), #3144, .T. ) ;
#1316 = AXIS2_PLACEMENT_3D ( 'NONE', #2410, #5655, #7606 ) ;
#1317 = AXIS2_PLACEMENT_3D ( 'NONE', #8097, #360, #4859 ) ;
#1318 = EDGE_CURVE ( 'NONE', #6647, #5567, #5729, .T. ) ;
#1319 = ORIENTED_EDGE ( 'NONE', *, *, #5004, .F. ) ;
#1320 = DIRECTION ( 'NONE',  ( -0.000000000000000000, 1.000000000000000000, -0.000000000000000000 ) ) ;
#1321 = FACE_BOUND ( 'NONE', #4122, .T. ) ;
#1322 = DIRECTION ( 'NONE',  ( -7.304098846218136639E-16, 0.000000000000000000, -1.000000000000000000 ) ) ;
#1323 = DIRECTION ( 'NONE',  ( 0.000000000000000000, 0.000000000000000000, 1.000000000000000000 ) ) ;
#1324 = STYLED_ITEM ( 'NONE', ( #109 ), #6657 ) ;
#1325 = VECTOR ( 'NONE', #254, 1000.000000000000000 ) ;
#1326 = CIRCLE ( 'NONE', #8075, 1.599999999999998979 ) ;
#1327 = PLANE ( 'NONE',  #8101 ) ;
#1328 = PRODUCT_DEFINITION ( 'UNKNOWN', '', #2448, #227 ) ;
#1329 = CARTESIAN_POINT ( 'NONE',  ( -39.00000000000000711, 85.00000000000017053, 5.000000000000045297 ) ) ;
#1330 = CIRCLE ( 'NONE', #2383, 0.2000000000000000944 ) ;
#1331 = ORIENTED_EDGE ( 'NONE', *, *, #179, .T. ) ;
#1332 = CIRCLE ( 'NONE', #2651, 1.280000000000000027 ) ;
#1333 = DIRECTION ( 'NONE',  ( -1.000000000000000000, 0.000000000000000000, 2.065146995210483462E-17 ) ) ;
#1334 = AXIS2_PLACEMENT_3D ( 'NONE', #7590, #3855, #1397 ) ;
#1335 = AXIS2_PLACEMENT_3D ( 'NONE', #2275, #4809, #5967 ) ;
#1336 = FACE_OUTER_BOUND ( 'NONE', #6727, .T. ) ;
#1337 = CARTESIAN_POINT ( 'NONE',  ( 9.020562075079396891E-14, 10.00000000000000000, 729.2499999999977263 ) ) ;
#1338 = CARTESIAN_POINT ( 'NONE',  ( -1.321505333908963742, 3.855830693249141738, -2.665789719053469398 ) ) ;
#1339 = DIRECTION ( 'NONE',  ( 1.000000000000000000, 0.000000000000000000, 0.000000000000000000 ) ) ;
#1340 = ADVANCED_FACE ( 'NONE', ( #7539 ), #22, .F. ) ;
#1341 = ORIENTED_EDGE ( 'NONE', *, *, #6915, .T. ) ;
#1343 = EDGE_CURVE ( 'NONE', #4949, #1038, #675, .T. ) ;
#1342 = VECTOR ( 'NONE', #7696, 1000.000000000000000 ) ;
#1344 = ORIENTED_EDGE ( 'NONE', *, *, #4461, .T. ) ;
#1345 = CARTESIAN_POINT ( 'NONE',  ( 0.000000000000000000, -1.478016689125442706, 1.843143693225357538E-15 ) ) ;
#1346 = ORIENTED_EDGE ( 'NONE', *, *, #4496, .F. ) ;
#1347 = ORIENTED_EDGE ( 'NONE', *, *, #6253, .T. ) ;
#1348 = CARTESIAN_POINT ( 'NONE',  ( 0.000000000000000000, 0.000000000000000000, -25.03750572909317285 ) ) ;
#1350 = EDGE_CURVE ( 'NONE', #4097, #5106, #4928, .T. ) ;
#1349 = LINE ( 'NONE', #1971, #5962 ) ;
#1351 = CARTESIAN_POINT ( 'NONE',  ( 1.257674520083185143E-14, 4.618802153517020948, -0.3572655899081733644 ) ) ;
#1352 = DIRECTION ( 'NONE',  ( 1.548532948139399967E-17, 0.000000000000000000, -1.000000000000000000 ) ) ;
#1353 = VECTOR ( 'NONE', #6533, 1000.000000000000000 ) ;
#1354 = ORIENTED_EDGE ( 'NONE', *, *, #3875, .F. ) ;
#1355 = ORIENTED_EDGE ( 'NONE', *, *, #5972, .T. ) ;
#1356 = EDGE_LOOP ( 'NONE', ( #3757, #2384 ) ) ;
#1357 = DIRECTION ( 'NONE',  ( 0.000000000000000000, 0.000000000000000000, 1.000000000000000000 ) ) ;
#1358 = CARTESIAN_POINT ( 'NONE',  ( 41.93162413031729585, 82.60433940584233881, -0.1928755069450422688 ) ) ;
#1359 = CYLINDRICAL_SURFACE ( 'NONE', #7664, 2.399999999999985256 ) ;
#1360 =( NAMED_UNIT ( * ) PLANE_ANGLE_UNIT ( ) SI_UNIT ( $, .RADIAN. ) );
#1361 = DIRECTION ( 'NONE',  ( -0.000000000000000000, -0.000000000000000000, 1.000000000000000000 ) ) ;
#1362 = MANIFOLD_SOLID_BREP ( 'Tap Drill for M4 Tap2', #4092 ) ;
#1363 = CIRCLE ( 'NONE', #815, 2.600000000000000089 ) ;
#1364 = DIRECTION ( 'NONE',  ( 0.000000000000000000, -0.000000000000000000, 1.000000000000000000 ) ) ;
#1365 = DIRECTION ( 'NONE',  ( 0.000000000000000000, 0.000000000000000000, 1.000000000000000000 ) ) ;
#1366 = DIRECTION ( 'NONE',  ( 1.000000000000000000, 0.000000000000000000, 0.000000000000000000 ) ) ;
#1367 = CARTESIAN_POINT ( 'NONE',  ( 0.000000000000000000, 0.000000000000000000, 0.000000000000000000 ) ) ;
#1368 = SHAPE_REPRESENTATION ( 'H_bar', ( #1587 ), #2170 ) ;
#1369 = EDGE_CURVE ( 'NONE', #6012, #4327, #5321, .T. ) ;
#1370 = EDGE_CURVE ( 'NONE', #5556, #3085, #2015, .T. ) ;
#1371 = CARTESIAN_POINT ( 'NONE',  ( -49.98886144361672734, 86.06516230458035466, 2.156352803700620768 ) ) ;
#1372 = AXIS2_PLACEMENT_3D ( 'NONE', #515, #4264, #3549 ) ;
#1373 = ORIENTED_EDGE ( 'NONE', *, *, #7808, .T. ) ;
#1374 = LINE ( 'NONE', #612, #1119 ) ;
#1375 =( REPRESENTATION_RELATIONSHIP ('NONE','NONE', #3916, #1368 ) REPRESENTATION_RELATIONSHIP_WITH_TRANSFORMATION ( #7145 )SHAPE_REPRESENTATION_RELATIONSHIP( ) );
#1376 = DIRECTION ( 'NONE',  ( 1.000000000000000000, 0.000000000000000000, -1.112002228190260397E-17 ) ) ;
#1377 = CARTESIAN_POINT ( 'NONE',  ( 52.00000000000000000, 7.999999999999996447, 11.99999999999998934 ) ) ;
#1378 = LINE ( 'NONE', #3393, #1984 ) ;
#1379 = SURFACE_SIDE_STYLE ('',( #7058 ) ) ;
#1380 = EDGE_LOOP ( 'NONE', ( #4374, #4573, #4787 ) ) ;
#1381 = ORIENTED_EDGE ( 'NONE', *, *, #725, .F. ) ;
#1382 = CARTESIAN_POINT ( 'NONE',  ( -39.99999999999999289, -39.99999999999999289, 10.00000000000000000 ) ) ;
#1383 = MECHANICAL_DESIGN_GEOMETRIC_PRESENTATION_REPRESENTATION (  '', ( #7478 ), #965 ) ;
#1384 = ORIENTED_EDGE ( 'NONE', *, *, #1760, .T. ) ;
#1385 = ORIENTED_EDGE ( 'NONE', *, *, #1137, .F. ) ;
#1386 = ADVANCED_FACE ( 'NONE', ( #1273 ), #6107, .T. ) ;
#1387 = EDGE_CURVE ( 'NONE', #3946, #4855, #388, .T. ) ;
#1388 = CARTESIAN_POINT ( 'NONE',  ( 2.000000000000000000, 1.773042676681340968, -2.276824562219559311E-15 ) ) ;
#1389 = CARTESIAN_POINT ( 'NONE',  ( -54.99999999999990052, -8.000000000000001776, 17.64999999999876579 ) ) ;
#1390 = FACE_BOUND ( 'NONE', #897, .T. ) ;
#1391 =( NAMED_UNIT ( * ) PLANE_ANGLE_UNIT ( ) SI_UNIT ( $, .RADIAN. ) );
#1392 = VERTEX_POINT ( 'NONE', #4706 ) ;
#1393 = ORIENTED_EDGE ( 'NONE', *, *, #6516, .T. ) ;
#1394 = ORIENTED_EDGE ( 'NONE', *, *, #4048, .T. ) ;
#1395 = EDGE_LOOP ( 'NONE', ( #5774, #472, #852, #846 ) ) ;
#1396 = DIRECTION ( 'NONE',  ( 0.000000000000000000, 0.000000000000000000, 1.000000000000000000 ) ) ;
#1397 = DIRECTION ( 'NONE',  ( 0.000000000000000000, 0.000000000000000000, 1.000000000000000000 ) ) ;
#1398 = LINE ( 'NONE', #7743, #5160 ) ;
#1399 = CARTESIAN_POINT ( 'NONE',  ( -3.094755790304997145, -6.282913975126477979, 8.006611220574070487 ) ) ;
#1400 = VECTOR ( 'NONE', #765, 1000.000000000000000 ) ;
#1401 = MANIFOLD_SOLID_BREP ( 'M3 Clearance Hole1', #6605 ) ;
#1402 = EDGE_CURVE ( 'NONE', #2014, #5401, #5202, .T. ) ;
#1403 = FACE_OUTER_BOUND ( 'NONE', #1036, .T. ) ;
#1404 = DIRECTION ( 'NONE',  ( -1.000000000000000000, -0.000000000000000000, -0.000000000000000000 ) ) ;
#1405 = CARTESIAN_POINT ( 'NONE',  ( 2.000000000000000000, 0.8865213383406723713, 1.535499999999998755 ) ) ;
#1406 = CARTESIAN_POINT ( 'NONE',  ( -49.94817596271295201, 87.27669880683387760, -0.7754554817172341075 ) ) ;
#1407 = ORIENTED_EDGE ( 'NONE', *, *, #303, .F. ) ;
#1408 = CARTESIAN_POINT ( 'NONE',  ( 2.000000000000000000, 0.000000000000000000, 0.000000000000000000 ) ) ;
#1409 = CARTESIAN_POINT ( 'NONE',  ( 2.000000000000027089, 3.464101615137739731, -2.700000000000001066 ) ) ;
#1410 = DIRECTION ( 'NONE',  ( 0.000000000000000000, 0.000000000000000000, -1.000000000000000000 ) ) ;
#1411 = CARTESIAN_POINT ( 'NONE',  ( 11.00000000000000355, 0.000000000000000000, 0.000000000000000000 ) ) ;
#1412 = DIRECTION ( 'NONE',  ( 0.000000000000000000, -0.5000000000000009992, -0.8660254037844380415 ) ) ;
#1413 = ORIENTED_EDGE ( 'NONE', *, *, #5740, .T. ) ;
#1414 = CARTESIAN_POINT ( 'NONE',  ( 5.000000000000015099, 0.000000000000000000, 0.000000000000000000 ) ) ;
#1415 = EDGE_LOOP ( 'NONE', ( #2634, #5708, #1140, #7987, #6582 ) ) ;
#1416 = ADVANCED_FACE ( 'NONE', ( #7818 ), #7120, .F. ) ;
#1417 = ORIENTED_EDGE ( 'NONE', *, *, #63, .F. ) ;
#1418 = ORIENTED_EDGE ( 'NONE', *, *, #2801, .F. ) ;
#1419 = VERTEX_POINT ( 'NONE', #5911 ) ;
#1420 = EDGE_CURVE ( 'NONE', #5767, #4437, #7892, .T. ) ;
#1421 = AXIS2_PLACEMENT_3D ( 'NONE', #4138, #4718, #1488 ) ;
#1422 = AXIS2_PLACEMENT_3D ( 'NONE', #1747, #5608, #1875 ) ;
#1423 = CARTESIAN_POINT ( 'NONE',  ( 52.00000000000000000, -8.000000000000003553, 11.99999999999998934 ) ) ;
#1424 = CARTESIAN_POINT ( 'NONE',  ( 4.000000000000003553, 2.309401076758480720, -2.700000000000000178 ) ) ;
#1425 = DIRECTION ( 'NONE',  ( -5.833327817117373438E-17, 1.000000000000000000, 1.363075293218192124E-18 ) ) ;
#1426 = MANIFOLD_SOLID_BREP ( 'Hex', #644 ) ;
#1427 = PRODUCT_DEFINITION ( 'UNKNOWN', '', #570, #1256 ) ;
#1428 = ORIENTED_EDGE ( 'NONE', *, *, #3937, .T. ) ;
#1429 = VERTEX_POINT ( 'NONE', #4670 ) ;
#1430 = EDGE_LOOP ( 'NONE', ( #2699, #674, #6368, #3754 ) ) ;
#1431 = CARTESIAN_POINT ( 'NONE',  ( 29.99999999999997868, 30.00000000000001421, 10.00000000000000000 ) ) ;
#1432 = CARTESIAN_POINT ( 'NONE',  ( 41.94112359463814954, 82.77568671679536294, -0.9366119428080386111 ) ) ;
#1433 = LINE ( 'NONE', #6562, #6338 ) ;
#1434 = PRESENTATION_STYLE_ASSIGNMENT (( #5798 ) ) ;
#1435 = SURFACE_STYLE_FILL_AREA ( #5298 ) ;
#1436 = AXIS2_PLACEMENT_3D ( 'NONE', #1181, #2518, #6869 ) ;
#1437 = STYLED_ITEM ( 'NONE', ( #3738 ), #6901 ) ;
#1438 = DIRECTION ( 'NONE',  ( 0.000000000000000000, 0.000000000000000000, 1.000000000000000000 ) ) ;
#1439 = CARTESIAN_POINT ( 'NONE',  ( 1.300000000000000044, 0.7390083445627193548, -1.280000000000000693 ) ) ;
#1440 =( NAMED_UNIT ( * ) SI_UNIT ( $, .STERADIAN. ) SOLID_ANGLE_UNIT ( ) );
#1441 = CIRCLE ( 'NONE', #7669, 4.250000000000000000 ) ;
#1442 = ADVANCED_FACE ( 'NONE', ( #2094 ), #6321, .F. ) ;
#1443 = LINE ( 'NONE', #5995, #2545 ) ;
#1444 = CIRCLE ( 'NONE', #5554, 1.249999999999998668 ) ;
#1445 = DIRECTION ( 'NONE',  ( -0.000000000000000000, 1.000000000000000000, -0.000000000000000000 ) ) ;
#1446 = AXIS2_PLACEMENT_3D ( 'NONE', #1208, #5779, #4320 ) ;
#1447 = EDGE_LOOP ( 'NONE', ( #6676, #192 ) ) ;
#1448 = CARTESIAN_POINT ( 'NONE',  ( 2.650000000000006573, 0.000000000000000000, 14.60000000000000142 ) ) ;
#1449 = AXIS2_PLACEMENT_3D ( 'NONE', #678, #2598, #5589 ) ;
#1450 =( NAMED_UNIT ( * ) PLANE_ANGLE_UNIT ( ) SI_UNIT ( $, .RADIAN. ) );
#1451 = CARTESIAN_POINT ( 'NONE',  ( -4.000000000000000000, -2.309401076758531346, -0.3572655899081733644 ) ) ;
#1452 = CIRCLE ( 'NONE', #2643, 7.000000000000000000 ) ;
#1453 = AXIS2_PLACEMENT_3D ( 'NONE', #7511, #3899, #5229 ) ;
#1454 = CARTESIAN_POINT ( 'NONE',  ( 1.257674520083185143E-14, 4.618802153517020948, -0.3572655899081733644 ) ) ;
#1455 = VECTOR ( 'NONE', #6425, 1000.000000000000000 ) ;
#1456 = CARTESIAN_POINT ( 'NONE',  ( 3.344563996438206122, 2.687817229851463097, -0.1586754815284832643 ) ) ;
#1457 = ORIENTED_EDGE ( 'NONE', *, *, #4882, .T. ) ;
#1458 = CARTESIAN_POINT ( 'NONE',  ( -4.000000000000000000, -2.309401076758531346, -2.342734410091827701 ) ) ;
#1459 = ORIENTED_EDGE ( 'NONE', *, *, #8079, .T. ) ;
#1460 = CIRCLE ( 'NONE', #2781, 2.200000000000001066 ) ;
#1461 = VERTEX_POINT ( 'NONE', #835 ) ;
#1462 = PLANE ( 'NONE',  #230 ) ;
#1463 = LINE ( 'NONE', #2826, #5036 ) ;
#1464 = DIRECTION ( 'NONE',  ( -0.8571673007021118895, -1.430919794933844670E-16, -0.5150380749100549327 ) ) ;
#1465 = APPLICATION_PROTOCOL_DEFINITION ( 'draft international standard', 'automotive_design', 1998, #1960 ) ;
#1466 = EDGE_CURVE ( 'NONE', #7254, #493, #7769, .T. ) ;
#1467 = CIRCLE ( 'NONE', #1198, 2.650000000000010125 ) ;
#1468 = ADVANCED_FACE ( 'NONE', ( #3420 ), #251, .T. ) ;
#1469 = EDGE_CURVE ( 'NONE', #3630, #3047, #962, .T. ) ;
#1470 = ORIENTED_EDGE ( 'NONE', *, *, #6913, .T. ) ;
#1471 = VECTOR ( 'NONE', #2210, 1000.000000000000000 ) ;
#1472 = EDGE_LOOP ( 'NONE', ( #4035, #5326 ) ) ;
#1473 = ORIENTED_EDGE ( 'NONE', *, *, #2612, .F. ) ;
#1474 = LINE ( 'NONE', #3414, #1049 ) ;
#1475 = FACE_OUTER_BOUND ( 'NONE', #3870, .T. ) ;
#1476 = CARTESIAN_POINT ( 'NONE',  ( 0.000000000000000000, 2.357898499370434386, -3.469446951953614189E-15 ) ) ;
#1477 = AXIS2_PLACEMENT_3D ( 'NONE', #3055, #4799, #7985 ) ;
#1478 = DIRECTION ( 'NONE',  ( 1.000000000000000000, 0.000000000000000000, 0.000000000000000000 ) ) ;
#1479 = CARTESIAN_POINT ( 'NONE',  ( 0.000000000000000000, 0.000000000000000000, -2.674599999999998978 ) ) ;
#1480 = CARTESIAN_POINT ( 'NONE',  ( 0.000000000000000000, 0.000000000000000000, -2.700000000000001066 ) ) ;
#1481 = DIRECTION ( 'NONE',  ( 1.412205397084881070E-17, -2.775557561562891967E-17, -1.000000000000000000 ) ) ;
#1482 = CYLINDRICAL_SURFACE ( 'NONE', #7579, 2.149999999999995470 ) ;
#1483 = DIRECTION ( 'NONE',  ( -1.000000000000000000, -1.502586498047605218E-16, 1.238733049487200360E-17 ) ) ;
#1484 = FACE_OUTER_BOUND ( 'NONE', #4253, .T. ) ;
#1485 = VERTEX_POINT ( 'NONE', #2875 ) ;
#1486 = DIRECTION ( 'NONE',  ( -1.000000000000000000, 0.000000000000000000, 0.000000000000000000 ) ) ;
#1487 =( NAMED_UNIT ( * ) PLANE_ANGLE_UNIT ( ) SI_UNIT ( $, .RADIAN. ) );
#1488 = DIRECTION ( 'NONE',  ( -1.000000000000000000, 0.000000000000000000, 0.000000000000000000 ) ) ;
#1489 = ADVANCED_FACE ( 'NONE', ( #4795 ), #6738, .F. ) ;
#1490 = DIRECTION ( 'NONE',  ( 0.000000000000000000, 0.000000000000000000, -1.000000000000000000 ) ) ;
#1491 = FILL_AREA_STYLE ('',( #774 ) ) ;
#1492 = VECTOR ( 'NONE', #1529, 1000.000000000000114 ) ;
#1493 = CARTESIAN_POINT ( 'NONE',  ( 2.500000000000002220, 2.357898499370434386, -3.469446951953614189E-15 ) ) ;
#1494 = VERTEX_POINT ( 'NONE', #2996 ) ;
#1495 = CARTESIAN_POINT ( 'NONE',  ( 1.300000000000000044, 1.478016689125442484, -1.626303258728256651E-15 ) ) ;
#1496 = UNCERTAINTY_MEASURE_WITH_UNIT (LENGTH_MEASURE( 1.000000000000000082E-05 ), #1674, 'distance_accuracy_value', 'NONE');
#1497 = ORIENTED_EDGE ( 'NONE', *, *, #7301, .T. ) ;
#1498 = ORIENTED_EDGE ( 'NONE', *, *, #8120, .T. ) ;
#1499 = CARTESIAN_POINT ( 'NONE',  ( 0.000000000000000000, -1.773042676681340968, 2.059984127722458425E-15 ) ) ;
#1500 = EDGE_CURVE ( 'NONE', #8121, #6469, #2961, .T. ) ;
#1501 = DIRECTION ( 'NONE',  ( 0.000000000000000000, 1.224646799147353207E-16, 1.000000000000000000 ) ) ;
#1502 = FACE_OUTER_BOUND ( 'NONE', #6197, .T. ) ;
#1503 = ORIENTED_EDGE ( 'NONE', *, *, #4756, .T. ) ;
#1504 = ORIENTED_EDGE ( 'NONE', *, *, #6628, .F. ) ;
#1505 = ORIENTED_EDGE ( 'NONE', *, *, #7848, .T. ) ;
#1506 = EDGE_CURVE ( 'NONE', #3838, #1494, #5542, .T. ) ;
#1507 = CARTESIAN_POINT ( 'NONE',  ( 58.00000000000000000, -8.000000000000000000, 0.000000000000000000 ) ) ;
#1508 = DIRECTION ( 'NONE',  ( -0.000000000000000000, -0.000000000000000000, 1.000000000000000000 ) ) ;
#1509 = CARTESIAN_POINT ( 'NONE',  ( 0.000000000000000000, 37.49999999999999289, 4.000000000000000000 ) ) ;
#1510 = STYLED_ITEM ( 'NONE', ( #7117 ), #886 ) ;
#1511 = SURFACE_STYLE_FILL_AREA ( #5296 ) ;
#1512 = DIRECTION ( 'NONE',  ( 1.412205397084881070E-17, -2.775557561562891967E-17, -1.000000000000000000 ) ) ;
#1513 = AXIS2_PLACEMENT_3D ( 'NONE', #1303, #5175, #5054 ) ;
#1514 = LINE ( 'NONE', #2716, #2239 ) ;
#1515 = DIRECTION ( 'NONE',  ( -1.000000000000000000, 0.000000000000000000, 0.000000000000000000 ) ) ;
#1516 =( NAMED_UNIT ( * ) SI_UNIT ( $, .STERADIAN. ) SOLID_ANGLE_UNIT ( ) );
#1517 = CARTESIAN_POINT ( 'NONE',  ( -59.99999999999999289, 85.00000000000045475, -1.387778780781445676E-14 ) ) ;
#1518 = CARTESIAN_POINT ( 'NONE',  ( 6.764948177723724143, 1.813303243961031264, 8.031723462610594666 ) ) ;
#1519 = EDGE_CURVE ( 'NONE', #8200, #5522, #2299, .T. ) ;
#1520 = ORIENTED_EDGE ( 'NONE', *, *, #669, .F. ) ;
#1521 = EDGE_CURVE ( 'NONE', #6523, #2846, #8020, .T. ) ;
#1522 = CARTESIAN_POINT ( 'NONE',  ( 0.000000000000000000, 0.000000000000000000, -0.2800830152838832965 ) ) ;
#1523 = CARTESIAN_POINT ( 'NONE',  ( 5.200000000000020606, 0.000000000000000000, -6.938893903907228378E-15 ) ) ;
#1524 = ADVANCED_FACE ( 'NONE', ( #7492 ), #3504, .F. ) ;
#1525 = LINE ( 'NONE', #4028, #869 ) ;
#1526 = CARTESIAN_POINT ( 'NONE',  ( 2.000000000000027089, 3.464101615137739731, 0.000000000000000000 ) ) ;
#1527 = DIRECTION ( 'NONE',  ( -1.000000000000000000, -0.000000000000000000, -0.000000000000000000 ) ) ;
#1528 = PLANE ( 'NONE',  #5581 ) ;
#1529 = DIRECTION ( 'NONE',  ( 0.000000000000000000, -0.5000000000000011102, -0.8660254037844379305 ) ) ;
#1530 = EDGE_LOOP ( 'NONE', ( #6903, #2912, #2180, #3251 ) ) ;
#1531 = CYLINDRICAL_SURFACE ( 'NONE', #5398, 3.500000000000000000 ) ;
#1532 = ORIENTED_EDGE ( 'NONE', *, *, #4413, .F. ) ;
#1533 = ORIENTED_EDGE ( 'NONE', *, *, #3542, .F. ) ;
#1534 = DIRECTION ( 'NONE',  ( 0.000000000000000000, 0.000000000000000000, 1.000000000000000000 ) ) ;
#1535 = CARTESIAN_POINT ( 'NONE',  ( 4.000000000000004441, -1.549102112939113152, -2.542104661404056554 ) ) ;
#1536 = LINE ( 'NONE', #6474, #4626 ) ;
#1537 = LINE ( 'NONE', #7107, #5041 ) ;
#1538 = PRODUCT_CONTEXT ( 'NONE', #2541, 'mechanical' ) ;
#1539 = EDGE_CURVE ( 'NONE', #4465, #1812, #6983, .T. ) ;
#1540 = ORIENTED_EDGE ( 'NONE', *, *, #920, .F. ) ;
#1541 = EDGE_CURVE ( 'NONE', #3673, #5642, #1677, .T. ) ;
#1542 = EDGE_LOOP ( 'NONE', ( #8150, #4247, #311, #2237, #5971 ) ) ;
#1543 = ORIENTED_EDGE ( 'NONE', *, *, #5800, .F. ) ;
#1544 = FACE_BOUND ( 'NONE', #3563, .T. ) ;
#1545 = CARTESIAN_POINT ( 'NONE',  ( -41.98520465537847457, 86.13165801428257851, 2.129342995125455662 ) ) ;
#1546 = DIRECTION ( 'NONE',  ( 0.000000000000000000, 0.000000000000000000, 1.000000000000000000 ) ) ;
#1547 = FILL_AREA_STYLE_COLOUR ( '', #2588 ) ;
#1548 = DIRECTION ( 'NONE',  ( -0.000000000000000000, -0.000000000000000000, -1.000000000000000000 ) ) ;
#1549 = DIRECTION ( 'NONE',  ( -1.000000000000000000, -0.000000000000000000, -0.000000000000000000 ) ) ;
#1550 = CARTESIAN_POINT ( 'NONE',  ( 4.200000000000001954, 0.000000000000000000, -2.200000000000001066 ) ) ;
#1551 = FILL_AREA_STYLE ('',( #6745 ) ) ;
#1552 = LINE ( 'NONE', #7780, #1353 ) ;
#1553 = ADVANCED_FACE ( 'NONE', ( #5418 ), #7935, .T. ) ;
#1554 = DIRECTION ( 'NONE',  ( -1.000000000000000000, -0.000000000000000000, -0.000000000000000000 ) ) ;
#1555 = VECTOR ( 'NONE', #5187, 1000.000000000000000 ) ;
#1556 = EDGE_CURVE ( 'NONE', #2129, #2623, #1668, .T. ) ;
#1557 = STYLED_ITEM ( 'NONE', ( #1912 ), #6918 ) ;
#1558 = ORIENTED_EDGE ( 'NONE', *, *, #6373, .F. ) ;
#1559 = ORIENTED_EDGE ( 'NONE', *, *, #7278, .F. ) ;
#1560 = DIRECTION ( 'NONE',  ( 0.000000000000000000, 0.000000000000000000, 1.000000000000000000 ) ) ;
#1561 = CONICAL_SURFACE ( 'NONE', #3019, 1.249999999999998002, 1.029744258676653645 ) ;
#1562 = DIRECTION ( 'NONE',  ( -7.304098846218136639E-16, 0.000000000000000000, -1.000000000000000000 ) ) ;
#1563 = DIRECTION ( 'NONE',  ( 0.000000000000000000, 0.000000000000000000, 1.000000000000000000 ) ) ;
#1564 = CARTESIAN_POINT ( 'NONE',  ( -2.000000000000022649, -3.464101615137742396, 0.000000000000000000 ) ) ;
#1565 = CARTESIAN_POINT ( 'NONE',  ( 55.00000000000000000, 10.00000000000000000, 17.65000000000000213 ) ) ;
#1566 = ADVANCED_FACE ( 'NONE', ( #1641 ), #6697, .F. ) ;
#1567 = FACE_OUTER_BOUND ( 'NONE', #6558, .T. ) ;
#1568 = CIRCLE ( 'NONE', #4360, 1.599999999999998979 ) ;
#1569 = CIRCLE ( 'NONE', #363, 50.00000000000002132 ) ;
#1570 = FACE_OUTER_BOUND ( 'NONE', #6194, .T. ) ;
#1571 = ORIENTED_EDGE ( 'NONE', *, *, #8156, .F. ) ;
#1572 = CARTESIAN_POINT ( 'NONE',  ( -31.74999999999995737, 0.000000000000000000, 1.500000000000000222 ) ) ;
#1573 = ORIENTED_EDGE ( 'NONE', *, *, #7711, .T. ) ;
#1574 = AXIS2_PLACEMENT_3D ( 'NONE', #7655, #6283, #1302 ) ;
#1575 = VERTEX_POINT ( 'NONE', #6120 ) ;
#1576 = CIRCLE ( 'NONE', #3308, 1.219500000000000028 ) ;
#1577 = FACE_OUTER_BOUND ( 'NONE', #5280, .T. ) ;
#1578 = DIRECTION ( 'NONE',  ( -1.000000000000000000, -0.000000000000000000, -0.000000000000000000 ) ) ;
#1579 = CIRCLE ( 'NONE', #5829, 42.00000000000002132 ) ;
#1580 = CARTESIAN_POINT ( 'NONE',  ( -29.99999999999999289, 30.00000000000000711, 10.00000000000000000 ) ) ;
#1581 = CARTESIAN_POINT ( 'NONE',  ( -5.560873836092222078, 4.276402017733387240, 8.021392354376160938 ) ) ;
#1582 = EDGE_CURVE ( 'NONE', #8109, #1110, #5914, .T. ) ;
#1583 = PLANE ( 'NONE',  #1844 ) ;
#1584 = SHAPE_DEFINITION_REPRESENTATION ( #5, #2201 ) ;
#1585 = ADVANCED_FACE ( 'NONE', ( #4332 ), #1131, .F. ) ;
#1586 = AXIS2_PLACEMENT_3D ( 'NONE', #5762, #637, #3188 ) ;
#1587 = AXIS2_PLACEMENT_3D ( 'NONE', #3942, #5152, #6454 ) ;
#1588 = ORIENTED_EDGE ( 'NONE', *, *, #3229, .F. ) ;
#1589 = CIRCLE ( 'NONE', #3192, 1.500000000000000222 ) ;
#1590 = ORIENTED_EDGE ( 'NONE', *, *, #596, .F. ) ;
#1591 = ORIENTED_EDGE ( 'NONE', *, *, #1184, .F. ) ;
#1592 = ADVANCED_FACE ( 'NONE', ( #5591 ), #1820, .T. ) ;
#1593 = CIRCLE ( 'NONE', #6223, 4.000000000000000000 ) ;
#1594 = PLANE ( 'NONE',  #2523 ) ;
#1595 = LINE ( 'NONE', #6561, #5721 ) ;
#1596 = AXIS2_PLACEMENT_3D ( 'NONE', #4588, #6490, #3345 ) ;
#1597 = PLANE ( 'NONE',  #7271 ) ;
#1598 = EDGE_CURVE ( 'NONE', #5786, #1081, #7237, .T. ) ;
#1599 = ORIENTED_EDGE ( 'NONE', *, *, #5839, .F. ) ;
#1600 = DIRECTION ( 'NONE',  ( -1.000000000000000000, 0.000000000000000000, 0.000000000000000000 ) ) ;
#1601 = CIRCLE ( 'NONE', #795, 39.00000000000002132 ) ;
#1602 = DIRECTION ( 'NONE',  ( -0.000000000000000000, -0.000000000000000000, 1.000000000000000000 ) ) ;
#1603 = DIRECTION ( 'NONE',  ( 0.000000000000000000, -0.000000000000000000, 1.000000000000000000 ) ) ;
#1604 = MECHANICAL_DESIGN_GEOMETRIC_PRESENTATION_REPRESENTATION (  '', ( #2792 ), #540 ) ;
#1605 = CARTESIAN_POINT ( 'NONE',  ( 0.000000000000000000, 0.000000000000000000, 0.000000000000000000 ) ) ;
#1606 = CARTESIAN_POINT ( 'NONE',  ( 0.000000000000000000, 5.051668046482844583E-16, -4.000000000000000000 ) ) ;
#1607 = LINE ( 'NONE', #7781, #1909 ) ;
#1608 = ORIENTED_EDGE ( 'NONE', *, *, #4702, .F. ) ;
#1609 = VERTEX_POINT ( 'NONE', #3092 ) ;
#1610 = DIRECTION ( 'NONE',  ( 1.000000000000000000, 0.000000000000000000, 0.000000000000000000 ) ) ;
#1611 = LINE ( 'NONE', #2935, #3551 ) ;
#1612 = CARTESIAN_POINT ( 'NONE',  ( 55.00000000000000000, 7.999999999999996447, 13.35000000000000853 ) ) ;
#1613 = LINE ( 'NONE', #7372, #4745 ) ;
#1614 = DIRECTION ( 'NONE',  ( -1.000000000000000000, -0.000000000000000000, -0.000000000000000000 ) ) ;
#1615 = CARTESIAN_POINT ( 'NONE',  ( -52.00000000000006395, -8.000000000000003553, 11.99999999999998934 ) ) ;
#1616 = DIRECTION ( 'NONE',  ( -1.000000000000000000, 0.000000000000000000, 0.000000000000000000 ) ) ;
#1617 = VERTEX_POINT ( 'NONE', #7791 ) ;
#1618 = CARTESIAN_POINT ( 'NONE',  ( 3.099999999999998757, 0.000000000000000000, 0.000000000000000000 ) ) ;
#1619 = EDGE_LOOP ( 'NONE', ( #7400, #7255, #2248, #689, #7018, #5429 ) ) ;
#1620 = ORIENTED_EDGE ( 'NONE', *, *, #5507, .F. ) ;
#1621 = CARTESIAN_POINT ( 'NONE',  ( 1.300000000000000044, 1.478016689125442484, -1.626303258728256651E-15 ) ) ;
#1622 = DIRECTION ( 'NONE',  ( 1.000000000000000000, 1.502586498047605218E-16, -1.412205397084881070E-17 ) ) ;
#1623 = LINE ( 'NONE', #8003, #4801 ) ;
#1624 = AXIS2_PLACEMENT_3D ( 'NONE', #1580, #2325, #7348 ) ;
#1625 = CARTESIAN_POINT ( 'NONE',  ( -7.000000000000000000, 0.4621588634683668206, 8.033969604113732288 ) ) ;
#1626 = DIRECTION ( 'NONE',  ( -0.000000000000000000, -0.000000000000000000, -1.000000000000000000 ) ) ;
#1627 = APPLICATION_PROTOCOL_DEFINITION ( 'draft international standard', 'automotive_design', 1998, #3234 ) ;
#1628 = AXIS2_PLACEMENT_3D ( 'NONE', #2103, #4640, #7863 ) ;
#1629 = ORIENTED_EDGE ( 'NONE', *, *, #1128, .T. ) ;
#1630 = EDGE_CURVE ( 'NONE', #7075, #7290, #71, .T. ) ;
#1631 = EDGE_CURVE ( 'NONE', #3615, #6597, #2117, .T. ) ;
#1632 = EDGE_LOOP ( 'NONE', ( #3081, #3214, #592, #225, #4957 ) ) ;
#1633 = ORIENTED_EDGE ( 'NONE', *, *, #6648, .T. ) ;
#1634 = EDGE_CURVE ( 'NONE', #3388, #3918, #4571, .T. ) ;
#1635 = EDGE_CURVE ( 'NONE', #992, #244, #7584, .T. ) ;
#1636 = CARTESIAN_POINT ( 'NONE',  ( 30.00000000000001066, -29.99999999999997868, 4.599999999999997868 ) ) ;
#1637 = CARTESIAN_POINT ( 'NONE',  ( 1.300000000000000044, 1.108512516844082141, 0.6399999999999991251 ) ) ;
#1638 = DIRECTION ( 'NONE',  ( -0.000000000000000000, -1.000000000000000000, -0.000000000000000000 ) ) ;
#1639 = SURFACE_SIDE_STYLE ('',( #6695 ) ) ;
#1640 = ORIENTED_EDGE ( 'NONE', *, *, #3292, .F. ) ;
#1641 = FACE_OUTER_BOUND ( 'NONE', #2635, .T. ) ;
#1642 = MECHANICAL_DESIGN_GEOMETRIC_PRESENTATION_REPRESENTATION (  '', ( #5233 ), #833 ) ;
#1643 = CARTESIAN_POINT ( 'NONE',  ( -32.64999999999999147, 30.00000000000000711, 1.734723475976807094E-15 ) ) ;
#1644 = DIRECTION ( 'NONE',  ( -0.000000000000000000, 1.000000000000000000, -0.000000000000000000 ) ) ;
#1645 = CARTESIAN_POINT ( 'NONE',  ( -6.290416253262643309, -3.105047250628316213, 8.027410178832276699 ) ) ;
#1646 = DIRECTION ( 'NONE',  ( -1.000000000000000000, -0.000000000000000000, -0.000000000000000000 ) ) ;
#1647 = EDGE_CURVE ( 'NONE', #7219, #5129, #1001, .T. ) ;
#1648 = ORIENTED_EDGE ( 'NONE', *, *, #84, .F. ) ;
#1649 = ORIENTED_EDGE ( 'NONE', *, *, #3329, .T. ) ;
#1650 =( NAMED_UNIT ( * ) SI_UNIT ( $, .STERADIAN. ) SOLID_ANGLE_UNIT ( ) );
#1651 = DIRECTION ( 'NONE',  ( -1.000000000000000000, -0.000000000000000000, -0.000000000000000000 ) ) ;
#1652 = CARTESIAN_POINT ( 'NONE',  ( -2.339468227445728576, -3.268109542640674547, -1.759456838036632033E-14 ) ) ;
#1653 = DIRECTION ( 'NONE',  ( 1.000000000000000000, 0.000000000000000000, 0.000000000000000000 ) ) ;
#1654 = CARTESIAN_POINT ( 'NONE',  ( -49.99423685432763875, 84.22705925652886094, -2.277573141052998462 ) ) ;
#1655 = EDGE_CURVE ( 'NONE', #7104, #7111, #5666, .T. ) ;
#1656 = LINE ( 'NONE', #348, #6654 ) ;
#1657 = EDGE_LOOP ( 'NONE', ( #1071, #737 ) ) ;
#1658 = CYLINDRICAL_SURFACE ( 'NONE', #5801, 1.649999999999995248 ) ;
#1659 = ORIENTED_EDGE ( 'NONE', *, *, #3995, .F. ) ;
#1660 = ORIENTED_EDGE ( 'NONE', *, *, #5235, .T. ) ;
#1661 = LINE ( 'NONE', #4990, #4757 ) ;
#1662 = FACE_BOUND ( 'NONE', #5496, .T. ) ;
#1663 = CARTESIAN_POINT ( 'NONE',  ( 55.00000000000000000, 10.00000000000000000, -4.499999999999986677 ) ) ;
#1664 = CARTESIAN_POINT ( 'NONE',  ( 2.000000000000000000, 0.000000000000000000, 0.000000000000000000 ) ) ;
#1665 = ADVANCED_FACE ( 'NONE', ( #2078 ), #1142, .T. ) ;
#1666 = EDGE_LOOP ( 'NONE', ( #5675, #5495 ) ) ;
#1667 = EDGE_CURVE ( 'NONE', #3249, #6523, #5197, .T. ) ;
#1668 = B_SPLINE_CURVE_WITH_KNOTS ( 'NONE', 3,
 ( #7322, #1810, #4835, #4294, #1047, #4875 ),
 .UNSPECIFIED., .F., .F.,
 ( 4, 2, 4 ),
 ( 0.006456566858647417445, 0.007625406818786684658, 0.008794246778925951871 ),
 .UNSPECIFIED. ) ;
#1669 = ORIENTED_EDGE ( 'NONE', *, *, #3413, .F. ) ;
#1670 = ORIENTED_EDGE ( 'NONE', *, *, #3650, .T. ) ;
#1671 = DIRECTION ( 'NONE',  ( 1.000000000000000000, 1.502586498047605218E-16, -1.412205397084881070E-17 ) ) ;
#1672 = CARTESIAN_POINT ( 'NONE',  ( -41.08716857408418122, 108.0000000000001990, -4.999999999999976907 ) ) ;
#1673 = DIRECTION ( 'NONE',  ( 1.000000000000000000, 0.000000000000000000, -0.000000000000000000 ) ) ;
#1674 =( LENGTH_UNIT ( ) NAMED_UNIT ( * ) SI_UNIT ( .MILLI., .METRE. ) );
#1675 = ADVANCED_FACE ( 'NONE', ( #3953 ), #1531, .T. ) ;
#1676 = ORIENTED_EDGE ( 'NONE', *, *, #1631, .F. ) ;
#1677 = LINE ( 'NONE', #6195, #742 ) ;
#1678 = VERTEX_POINT ( 'NONE', #2154 ) ;
#1679 = CARTESIAN_POINT ( 'NONE',  ( 2.000000000000000000, -0.8865213383406685965, 1.535500000000000531 ) ) ;
#1680 = DIRECTION ( 'NONE',  ( 1.000000000000000000, 0.000000000000000000, 0.000000000000000000 ) ) ;
#1681 = VECTOR ( 'NONE', #5239, 1000.000000000000000 ) ;
#1682 = AXIS2_PLACEMENT_3D ( 'NONE', #4853, #2353, #4946 ) ;
#1683 =( NAMED_UNIT ( * ) SI_UNIT ( $, .STERADIAN. ) SOLID_ANGLE_UNIT ( ) );
#1684 = EDGE_CURVE ( 'NONE', #2291, #7441, #7253, .T. ) ;
#1685 = CARTESIAN_POINT ( 'NONE',  ( 6.282784822387311507, 3.095002094042488050, 8.027357021320174368 ) ) ;
#1686 = ORIENTED_EDGE ( 'NONE', *, *, #309, .T. ) ;
#1687 = ORIENTED_EDGE ( 'NONE', *, *, #7096, .T. ) ;
#1688 = EDGE_CURVE ( 'NONE', #2560, #7228, #6096, .T. ) ;
#1689 = CARTESIAN_POINT ( 'NONE',  ( 3.344563996438205677, 2.687817229851463097, -2.541324518471518079 ) ) ;
#1690 = DIRECTION ( 'NONE',  ( -0.000000000000000000, -1.000000000000000000, -0.000000000000000000 ) ) ;
#1691 = DIRECTION ( 'NONE',  ( -0.000000000000000000, -0.000000000000000000, 1.000000000000000000 ) ) ;
#1692 = CARTESIAN_POINT ( 'NONE',  ( -41.97904239022133055, 86.32664991614245764, 2.000000000000043521 ) ) ;
#1693 = AXIS2_PLACEMENT_3D ( 'NONE', #1509, #7116, #2715 ) ;
#1694 = FACE_OUTER_BOUND ( 'NONE', #2539, .T. ) ;
#1695 = EDGE_LOOP ( 'NONE', ( #6559, #7035 ) ) ;
#1696 = CIRCLE ( 'NONE', #7392, 2.750000000000000000 ) ;
#1697 = DIRECTION ( 'NONE',  ( -1.000000000000000000, -0.000000000000000000, -0.000000000000000000 ) ) ;
#1698 = ORIENTED_EDGE ( 'NONE', *, *, #1058, .T. ) ;
#1699 = ORIENTED_EDGE ( 'NONE', *, *, #1760, .F. ) ;
#1700 = VECTOR ( 'NONE', #5315, 1000.000000000000000 ) ;
#1701 = CARTESIAN_POINT ( 'NONE',  ( 1.321505333908969293, -3.855830693249185703, -0.03421028094655650942 ) ) ;
#1702 = CARTESIAN_POINT ( 'NONE',  ( 2.000000000000000000, -1.773042676681340524, 1.734723475976807094E-15 ) ) ;
#1703 = CARTESIAN_POINT ( 'NONE',  ( -24.99999999999999289, 30.00000000000000711, 10.00000000000000000 ) ) ;
#1704 = VECTOR ( 'NONE', #6343, 1000.000000000000000 ) ;
#1705 = DIRECTION ( 'NONE',  ( -1.000000000000000000, -0.000000000000000000, -0.000000000000000000 ) ) ;
#1706 = LINE ( 'NONE', #4240, #4219 ) ;
#1707 = CLOSED_SHELL ( 'NONE', ( #1053, #6857, #3744, #7849, #52, #3177, #8013, #7380, #2542, #877, #4577, #6237, #6128, #1489, #7472, #6294, #5255, #4884, #6339, #7045, #4476, #401, #6557, #1004, #4173, #5121, #2135, #4084, #4825, #4518, #2590, #7192, #5543, #7520, #3570, #2344, #5990 ) ) ;
#1708 = CIRCLE ( 'NONE', #1312, 2.000000000000000888 ) ;
#1709 = VECTOR ( 'NONE', #7695, 1000.000000000000000 ) ;
#1710 = ORIENTED_EDGE ( 'NONE', *, *, #2840, .T. ) ;
#1711 = EDGE_LOOP ( 'NONE', ( #4384, #23, #2821 ) ) ;
#1712 = EDGE_LOOP ( 'NONE', ( #5973, #1590 ) ) ;
#1713 = PLANE ( 'NONE',  #3048 ) ;
#1714 = ADVANCED_FACE ( 'NONE', ( #7304 ), #5443, .T. ) ;
#1715 = CARTESIAN_POINT ( 'NONE',  ( 4.199999999999995737, 0.000000000000000000, 0.000000000000000000 ) ) ;
#1716 = CARTESIAN_POINT ( 'NONE',  ( 0.000000000000000000, 0.000000000000000000, -8.000000000000000000 ) ) ;
#1717 = AXIS2_PLACEMENT_3D ( 'NONE', #732, #5741, #1376 ) ;
#1718 = UNCERTAINTY_MEASURE_WITH_UNIT (LENGTH_MEASURE( 1.000000000000000082E-05 ), #4596, 'distance_accuracy_value', 'NONE');
#1719 = VECTOR ( 'NONE', #4707, 1000.000000000000000 ) ;
#1720 = PRESENTATION_STYLE_ASSIGNMENT (( #4203 ) ) ;
#1721 = CIRCLE ( 'NONE', #7023, 2.750000000000000000 ) ;
#1722 = EDGE_CURVE ( 'NONE', #7485, #3458, #4689, .T. ) ;
#1723 = EDGE_CURVE ( 'NONE', #7610, #1891, #350, .T. ) ;
#1724 = ORIENTED_EDGE ( 'NONE', *, *, #2446, .T. ) ;
#1725 = CARTESIAN_POINT ( 'NONE',  ( 0.000000000000000000, 0.000000000000000000, 0.000000000000000000 ) ) ;
#1726 = AXIS2_PLACEMENT_3D ( 'NONE', #5818, #5131, #6438 ) ;
#1727 = VERTEX_POINT ( 'NONE', #2899 ) ;
#1728 = ORIENTED_EDGE ( 'NONE', *, *, #3275, .T. ) ;
#1729 = AXIS2_PLACEMENT_3D ( 'NONE', #3931, #5677, #1396 ) ;
#1730 = CONICAL_SURFACE ( 'NONE', #1051, 1.219500000000000028, 0.7853981633974680410 ) ;
#1731 = DIRECTION ( 'NONE',  ( 1.000000000000000000, 0.000000000000000000, 0.000000000000000000 ) ) ;
#1732 = CARTESIAN_POINT ( 'NONE',  ( -41.96471864142489494, 83.27150586048362868, 1.684781847096441298 ) ) ;
#1733 =( NAMED_UNIT ( * ) SI_UNIT ( $, .STERADIAN. ) SOLID_ANGLE_UNIT ( ) );
#1734 = PRESENTATION_STYLE_ASSIGNMENT (( #6788 ) ) ;
#1735 = AXIS2_PLACEMENT_3D ( 'NONE', #4329, #1845, #3539 ) ;
#1736 = PLANE ( 'NONE',  #1372 ) ;
#1737 = EDGE_CURVE ( 'NONE', #1769, #4916, #940, .T. ) ;
#1738 = VERTEX_POINT ( 'NONE', #7216 ) ;
#1739 = AXIS2_PLACEMENT_3D ( 'NONE', #6960, #7592, #688 ) ;
#1740 = VERTEX_POINT ( 'NONE', #894 ) ;
#1741 = CARTESIAN_POINT ( 'NONE',  ( 3.999999999999989786, -2.309401076758547777, -0.3572655899081733644 ) ) ;
#1742 = CYLINDRICAL_SURFACE ( 'NONE', #223, 2.399999999999985256 ) ;
#1743 = DIRECTION ( 'NONE',  ( 1.000000000000000000, 0.000000000000000000, -1.734723475976807094E-16 ) ) ;
#1744 = DIRECTION ( 'NONE',  ( 1.412205397084881070E-17, -2.775557561562891967E-17, -1.000000000000000000 ) ) ;
#1745 = AXIS2_PLACEMENT_3D ( 'NONE', #1367, #5806, #101 ) ;
#1746 = CARTESIAN_POINT ( 'NONE',  ( 4.199999999999995737, 2.694222958124178486E-16, 2.200000000000001066 ) ) ;
#1747 = CARTESIAN_POINT ( 'NONE',  ( 3.099999999999998757, 1.959434878635765477E-16, 1.600000000000000311 ) ) ;
#1748 = ORIENTED_EDGE ( 'NONE', *, *, #3669, .T. ) ;
#1749 = ORIENTED_EDGE ( 'NONE', *, *, #2036, .T. ) ;
#1750 = EDGE_CURVE ( 'NONE', #3287, #2510, #6633, .T. ) ;
#1751 = CARTESIAN_POINT ( 'NONE',  ( 29.99999999999997868, 30.00000000000001421, 1.734723475976807094E-15 ) ) ;
#1752 = CARTESIAN_POINT ( 'NONE',  ( 4.000000000000003553, 2.309401076758524685, -2.342734410091827701 ) ) ;
#1753 = CARTESIAN_POINT ( 'NONE',  ( 52.00000000000000711, -8.000000000000000000, -8.000000000000000000 ) ) ;
#1754 = CARTESIAN_POINT ( 'NONE',  ( -4.000000000000000000, -0.7779732554280791579, -0.03354435108167821283 ) ) ;
#1755 = CARTESIAN_POINT ( 'NONE',  ( 0.2500000000000002220, 0.000000000000000000, 2.081668171172168513E-14 ) ) ;
#1756 = CARTESIAN_POINT ( 'NONE',  ( 49.94311118432961649, 87.38465289139496406, -0.3128412141714160266 ) ) ;
#1757 = ORIENTED_EDGE ( 'NONE', *, *, #1805, .F. ) ;
#1758 = ORIENTED_EDGE ( 'NONE', *, *, #3166, .T. ) ;
#1759 = ORIENTED_EDGE ( 'NONE', *, *, #8046, .F. ) ;
#1760 = EDGE_CURVE ( 'NONE', #3458, #3935, #6566, .T. ) ;
#1761 = ORIENTED_EDGE ( 'NONE', *, *, #6798, .F. ) ;
#1762 = DIRECTION ( 'NONE',  ( 1.412205397084881070E-17, -2.775557561562891967E-17, -1.000000000000000000 ) ) ;
#1763 = CARTESIAN_POINT ( 'NONE',  ( 25.00000000000001421, -29.99999999999997868, 10.00000000000000000 ) ) ;
#1764 = FACE_OUTER_BOUND ( 'NONE', #2988, .T. ) ;
#1765 = CIRCLE ( 'NONE', #3887, 4.999999999999993783 ) ;
#1766 = EDGE_LOOP ( 'NONE', ( #6011, #2056, #6689, #6810, #2371 ) ) ;
#1767 = DIRECTION ( 'NONE',  ( -1.000000000000000000, 0.000000000000000000, 2.065146995210483462E-17 ) ) ;
#1768 = ORIENTED_EDGE ( 'NONE', *, *, #5700, .F. ) ;
#1769 = VERTEX_POINT ( 'NONE', #982 ) ;
#1770 = EDGE_CURVE ( 'NONE', #3287, #5411, #4813, .T. ) ;
#1771 = CARTESIAN_POINT ( 'NONE',  ( -54.99999999999990052, 10.00000000000000000, 15.49999999999877254 ) ) ;
#1772 = CARTESIAN_POINT ( 'NONE',  ( -41.97210380486418302, 83.46605959390291218, -1.850206309317909303 ) ) ;
#1773 = FACE_OUTER_BOUND ( 'NONE', #6146, .T. ) ;
#1774 = CARTESIAN_POINT ( 'NONE',  ( 9.020562070449730010E-14, 7.000000000000000000, 8.000000000000058620 ) ) ;
#1775 = ORIENTED_EDGE ( 'NONE', *, *, #2547, .F. ) ;
#1776 = VERTEX_POINT ( 'NONE', #5361 ) ;
#1777 = CARTESIAN_POINT ( 'NONE',  ( 1.599999999999992983, 37.49999999999999289, 4.000000000000000000 ) ) ;
#1778 = CARTESIAN_POINT ( 'NONE',  ( -39.99999999999999289, -39.99999999999999289, 0.000000000000000000 ) ) ;
#1779 = PLANE ( 'NONE',  #5951 ) ;
#1780 = DIRECTION ( 'NONE',  ( 0.000000000000000000, 1.000000000000000000, -0.000000000000000000 ) ) ;
#1781 = CARTESIAN_POINT ( 'NONE',  ( 0.000000000000000000, 0.000000000000000000, -0.3080913168122707546 ) ) ;
#1782 = PRODUCT_DEFINITION ( 'UNKNOWN', '', #2577, #5093 ) ;
#1783 = CARTESIAN_POINT ( 'NONE',  ( 2.000000000000000000, 1.773042676681340968, -2.276824562219559311E-15 ) ) ;
#1784 = EDGE_CURVE ( 'NONE', #2291, #480, #7179, .T. ) ;
#1785 = ADVANCED_FACE ( 'NONE', ( #7339 ), #1658, .F. ) ;
#1786 = ORIENTED_EDGE ( 'NONE', *, *, #4520, .T. ) ;
#1787 = ORIENTED_EDGE ( 'NONE', *, *, #2211, .F. ) ;
#1788 = COLOUR_RGB ( '', 0.08235294, 0.09019608, 0.10196078) ;
#1789 = CARTESIAN_POINT ( 'NONE',  ( 2.000000000000000000, 0.000000000000000000, 0.000000000000000000 ) ) ;
#1790 = DIRECTION ( 'NONE',  ( -1.000000000000000000, -0.000000000000000000, -0.000000000000000000 ) ) ;
#1791 = LINE ( 'NONE', #4318, #6747 ) ;
#1792 = CARTESIAN_POINT ( 'NONE',  ( -39.00000000000000711, 85.00000000000017053, 2.000000000000043965 ) ) ;
#1793 = DIRECTION ( 'NONE',  ( -1.412205397084881070E-17, 2.775557561562891967E-17, 1.000000000000000000 ) ) ;
#1794 = DIRECTION ( 'NONE',  ( 0.000000000000000000, -0.5000000000000008882, -0.8660254037844380415 ) ) ;
#1795 = CONTEXT_DEPENDENT_SHAPE_REPRESENTATION ( #6699, #4172 ) ;
#1796 = AXIS2_PLACEMENT_3D ( 'NONE', #1751, #6803, #7675 ) ;
#1797 = ORIENTED_EDGE ( 'NONE', *, *, #4018, .F. ) ;
#1798 =( REPRESENTATION_RELATIONSHIP ('NONE','NONE', #3916, #6987 ) REPRESENTATION_RELATIONSHIP_WITH_TRANSFORMATION ( #826 )SHAPE_REPRESENTATION_RELATIONSHIP( ) );
#1799 = EDGE_LOOP ( 'NONE', ( #3663, #273, #7586, #8140, #3207 ) ) ;
#1800 = EDGE_LOOP ( 'NONE', ( #1919, #2477, #6514, #4664 ) ) ;
#1801 = ORIENTED_EDGE ( 'NONE', *, *, #3973, .T. ) ;
#1802 = PRODUCT_DEFINITION_SHAPE ( 'NONE', 'NONE',  #1328 ) ;
#1803 = DIRECTION ( 'NONE',  ( 0.000000000000000000, -0.5000000000000009992, -0.8660254037844380415 ) ) ;
#1805 = EDGE_CURVE ( 'NONE', #7038, #6853, #6010, .T. ) ;
#1804 = CARTESIAN_POINT ( 'NONE',  ( -1.198153218366585720E-14, 42.68016229225776925, 4.000000000000001776 ) ) ;
#1806 = CARTESIAN_POINT ( 'NONE',  ( -2.999999999999998668, 35.09008114612887397, 4.000000000000000000 ) ) ;
#1807 = SHAPE_REPRESENTATION_RELATIONSHIP ( 'NONE' , 'NONE' ,  #1314, #7232 ) ;
#1808 = ORIENTED_EDGE ( 'NONE', *, *, #3629, .T. ) ;
#1809 = EDGE_CURVE ( 'NONE', #583, #4585, #5397, .T. ) ;
#1810 = CARTESIAN_POINT ( 'NONE',  ( 4.000000000000003553, 0.3904826640788058301, -2.020173579201506309E-15 ) ) ;
#1811 = ORIENTED_EDGE ( 'NONE', *, *, #2057, .F. ) ;
#1812 = VERTEX_POINT ( 'NONE', #4186 ) ;
#1813 = CARTESIAN_POINT ( 'NONE',  ( -3.469446951953613006E-15, 0.000000000000000000, 14.60000000000000142 ) ) ;
#1814 = CARTESIAN_POINT ( 'NONE',  ( -41.93240078214817856, 82.61791640338877585, 0.3192077737422600037 ) ) ;
#1815 = CARTESIAN_POINT ( 'NONE',  ( -54.99999999999990052, -10.00000000000000000, 13.34999999999877929 ) ) ;
#1816 =( NAMED_UNIT ( * ) PLANE_ANGLE_UNIT ( ) SI_UNIT ( $, .RADIAN. ) );
#1817 = CARTESIAN_POINT ( 'NONE',  ( 2.468988737128785083, 6.554131952896964819, 8.004194855151794741 ) ) ;
#1818 = ORIENTED_EDGE ( 'NONE', *, *, #6302, .F. ) ;
#1819 = ORIENTED_EDGE ( 'NONE', *, *, #2756, .T. ) ;
#1820 = CONICAL_SURFACE ( 'NONE', #3276, 4.000000000000000000, 1.047197551196595855 ) ;
#1821 = DIRECTION ( 'NONE',  ( -1.000000000000000000, 0.000000000000000000, 1.032573497605241731E-17 ) ) ;
#1822 = CARTESIAN_POINT ( 'NONE',  ( -39.83716857408418122, 108.0000000000001421, 4.163336342344337027E-14 ) ) ;
#1823 = ADVANCED_FACE ( 'NONE', ( #6716 ), #226, .T. ) ;
#1824 = DIRECTION ( 'NONE',  ( -0.000000000000000000, -0.000000000000000000, -1.000000000000000000 ) ) ;
#1825 = FACE_OUTER_BOUND ( 'NONE', #4648, .T. ) ;
#1826 = EDGE_CURVE ( 'NONE', #1171, #7228, #4333, .T. ) ;
#1827 = FACE_OUTER_BOUND ( 'NONE', #2336, .T. ) ;
#1828 = EDGE_LOOP ( 'NONE', ( #2953, #1676, #6166, #1174 ) ) ;
#1829 = DIRECTION ( 'NONE',  ( 1.000000000000000000, 0.000000000000000000, 0.000000000000000000 ) ) ;
#1830 = CARTESIAN_POINT ( 'NONE',  ( 35.00000000000000000, -29.99999999999997868, 10.00000000000000000 ) ) ;
#1831 = LINE ( 'NONE', #2451, #7552 ) ;
#1832 = CARTESIAN_POINT ( 'NONE',  ( -3.469446951953613006E-15, 0.000000000000000000, 14.60000000000000142 ) ) ;
#1833 = DIRECTION ( 'NONE',  ( 0.000000000000000000, -0.4999999999999991118, 0.8660254037844390407 ) ) ;
#1834 = CARTESIAN_POINT ( 'NONE',  ( 49.99422766321050204, 85.77334557296516948, 2.277359159638543851 ) ) ;
#1835 = CONTEXT_DEPENDENT_SHAPE_REPRESENTATION ( #3163, #3652 ) ;
#1836 = ORIENTED_EDGE ( 'NONE', *, *, #7656, .F. ) ;
#1837 = VECTOR ( 'NONE', #2638, 1000.000000000000000 ) ;
#1838 = EDGE_LOOP ( 'NONE', ( #7912, #4288, #1384, #3235, #6147 ) ) ;
#1839 = AXIS2_PLACEMENT_3D ( 'NONE', #3556, #4717, #885 ) ;
#1840 = ORIENTED_EDGE ( 'NONE', *, *, #1277, .F. ) ;
#1841 = ORIENTED_EDGE ( 'NONE', *, *, #5379, .F. ) ;
#1842 = EDGE_CURVE ( 'NONE', #4940, #5103, #3404, .T. ) ;
#1843 = CARTESIAN_POINT ( 'NONE',  ( 58.00000000000000000, -8.000000000000000000, 0.000000000000000000 ) ) ;
#1844 = AXIS2_PLACEMENT_3D ( 'NONE', #5980, #279, #7312 ) ;
#1845 = DIRECTION ( 'NONE',  ( 1.000000000000000000, 0.000000000000000000, 0.000000000000000000 ) ) ;
#1846 = EDGE_CURVE ( 'NONE', #5782, #2794, #8037, .T. ) ;
#1847 = DIRECTION ( 'NONE',  ( -0.000000000000000000, -0.000000000000000000, -1.000000000000000000 ) ) ;
#1848 = DIRECTION ( 'NONE',  ( 0.000000000000000000, 1.000000000000000000, 0.000000000000000000 ) ) ;
#1849 = CIRCLE ( 'NONE', #3840, 2.750000000000000000 ) ;
#1850 = AXIS2_PLACEMENT_3D ( 'NONE', #1970, #4420, #2016 ) ;
#1851 = ORIENTED_EDGE ( 'NONE', *, *, #6508, .F. ) ;
#1852 = CARTESIAN_POINT ( 'NONE',  ( 20.00000000000000355, 0.000000000000000000, 0.000000000000000000 ) ) ;
#1853 = ORIENTED_EDGE ( 'NONE', *, *, #434, .T. ) ;
#1854 = EDGE_CURVE ( 'NONE', #452, #2779, #609, .T. ) ;
#1855 = VERTEX_POINT ( 'NONE', #5521 ) ;
#1856 = AXIS2_PLACEMENT_3D ( 'NONE', #7030, #1936, #3040 ) ;
#1857 = VECTOR ( 'NONE', #3657, 1000.000000000000000 ) ;
#1858 = EDGE_CURVE ( 'NONE', #2626, #5387, #2479, .T. ) ;
#1859 = CIRCLE ( 'NONE', #7021, 4.999999999999993783 ) ;
#1861 = CARTESIAN_POINT ( 'NONE',  ( -42.00000000000000711, 85.00000000000046896, 2.399999999999971045 ) ) ;
#1860 = CIRCLE ( 'NONE', #907, 4.000000000000000000 ) ;
#1862 = CARTESIAN_POINT ( 'NONE',  ( 11.00000000000000355, 1.219500000000000028, 0.000000000000000000 ) ) ;
#1863 = DIRECTION ( 'NONE',  ( 1.000000000000000000, 0.000000000000000000, 0.000000000000000000 ) ) ;
#1864 = DIRECTION ( 'NONE',  ( 1.000000000000000000, 2.775557561562890365E-16, -1.734723475976806478E-17 ) ) ;
#1865 = CARTESIAN_POINT ( 'NONE',  ( 3.506487216771620563, 6.075720677264023095, 8.008423154362855456 ) ) ;
#1866 = VECTOR ( 'NONE', #6956, 1000.000000000000114 ) ;
#1867 = ORIENTED_EDGE ( 'NONE', *, *, #5059, .T. ) ;
#1868 = EDGE_LOOP ( 'NONE', ( #6268, #1910, #893, #6773 ) ) ;
#1869 = DIRECTION ( 'NONE',  ( 1.000000000000000000, 0.000000000000000000, 0.000000000000000000 ) ) ;
#1870 = CYLINDRICAL_SURFACE ( 'NONE', #5302, 39.00000000000002132 ) ;
#1871 = CARTESIAN_POINT ( 'NONE',  ( 0.000000000000000000, 0.000000000000000000, -2.700000000000001066 ) ) ;
#1872 = AXIS2_PLACEMENT_3D ( 'NONE', #4684, #3801, #5668 ) ;
#1873 = VECTOR ( 'NONE', #1744, 1000.000000000000000 ) ;
#1874 = FACE_OUTER_BOUND ( 'NONE', #2733, .T. ) ;
#1875 = DIRECTION ( 'NONE',  ( 0.000000000000000000, 1.224646799147353207E-16, 1.000000000000000000 ) ) ;
#1876 = PRODUCT ( 'V_bar', 'V_bar', '', ( #2708 ) ) ;
#1877 = AXIS2_PLACEMENT_3D ( 'NONE', #6386, #5148, #601 ) ;
#1878 = TOROIDAL_SURFACE ( 'NONE', #136, 2.200000000000001066, 0.2000000000000000111 ) ;
#1879 = ORIENTED_EDGE ( 'NONE', *, *, #7922, .T. ) ;
#1880 = CARTESIAN_POINT ( 'NONE',  ( -58.00000000000006395, -8.000000000000003553, 19.99999999999998934 ) ) ;
#1881 = CARTESIAN_POINT ( 'NONE',  ( -4.000000000000000000, -2.309401076758531346, -2.342734410091827701 ) ) ;
#1882 = CARTESIAN_POINT ( 'NONE',  ( 2.500000000000002220, 0.000000000000000000, 0.000000000000000000 ) ) ;
#1883 = CIRCLE ( 'NONE', #4931, 1.280000000000000027 ) ;
#1884 = DIRECTION ( 'NONE',  ( 0.000000000000000000, -1.000000000000000000, 1.222984857324291014E-15 ) ) ;
#1885 = DIRECTION ( 'NONE',  ( -0.000000000000000000, -0.000000000000000000, -1.000000000000000000 ) ) ;
#1886 = ORIENTED_EDGE ( 'NONE', *, *, #1519, .T. ) ;
#1887 = EDGE_LOOP ( 'NONE', ( #7113, #3158, #1286, #7615 ) ) ;
#1888 = CARTESIAN_POINT ( 'NONE',  ( 41.97904239022140160, 83.67335008385828132, 2.000000000000015543 ) ) ;
#1889 = EDGE_CURVE ( 'NONE', #2122, #6951, #1007, .T. ) ;
#1890 = ORIENTED_EDGE ( 'NONE', *, *, #2741, .T. ) ;
#1891 = VERTEX_POINT ( 'NONE', #439 ) ;
#1892 = FACE_OUTER_BOUND ( 'NONE', #1223, .T. ) ;
#1893 = DIRECTION ( 'NONE',  ( -0.000000000000000000, -0.000000000000000000, 1.000000000000000000 ) ) ;
#1894 = DIRECTION ( 'NONE',  ( -1.000000000000000000, 0.000000000000000000, 0.000000000000000000 ) ) ;
#1895 = CARTESIAN_POINT ( 'NONE',  ( 39.83716857408417411, 124.0119620251982582, 12.00000000000001776 ) ) ;
#1896 = ORIENTED_EDGE ( 'NONE', *, *, #1842, .F. ) ;
#1897 = CARTESIAN_POINT ( 'NONE',  ( 49.96737414687255097, 83.19055800108181131, 1.584620125915989775 ) ) ;
#1898 = EDGE_CURVE ( 'NONE', #3553, #3165, #6330, .T. ) ;
#1899 = VERTEX_POINT ( 'NONE', #3017 ) ;
#1900 = EDGE_CURVE ( 'NONE', #7604, #5220, #7469, .T. ) ;
#1901 = ADVANCED_FACE ( 'NONE', ( #7508 ), #2404, .F. ) ;
#1902 = ORIENTED_EDGE ( 'NONE', *, *, #2805, .T. ) ;
#1903 = DIRECTION ( 'NONE',  ( 0.000000000000000000, 0.000000000000000000, -1.000000000000000000 ) ) ;
#1904 = CARTESIAN_POINT ( 'NONE',  ( 41.96864087686234512, 83.36448938425077415, -1.774759388939936899 ) ) ;
#1905 = DIRECTION ( 'NONE',  ( 0.000000000000000000, -1.000000000000000000, 0.000000000000000000 ) ) ;
#1906 = AXIS2_PLACEMENT_3D ( 'NONE', #2824, #7310, #276 ) ;
#1907 = PRESENTATION_STYLE_ASSIGNMENT (( #723 ) ) ;
#1908 = LINE ( 'NONE', #3776, #6937 ) ;
#1909 = VECTOR ( 'NONE', #6570, 1000.000000000000000 ) ;
#1910 = ORIENTED_EDGE ( 'NONE', *, *, #5481, .T. ) ;
#1911 = ORIENTED_EDGE ( 'NONE', *, *, #6672, .F. ) ;
#1912 = PRESENTATION_STYLE_ASSIGNMENT (( #4890 ) ) ;
#1913 = FACE_OUTER_BOUND ( 'NONE', #159, .T. ) ;
#1914 = CARTESIAN_POINT ( 'NONE',  ( 2.000000000000000000, -0.8865213383406685965, 1.535500000000000531 ) ) ;
#1915 = FACE_OUTER_BOUND ( 'NONE', #1189, .T. ) ;
#1916 = CARTESIAN_POINT ( 'NONE',  ( 1.300000000000000044, -0.7390083445627200209, 1.280000000000001137 ) ) ;
#1917 = DIRECTION ( 'NONE',  ( 1.000000000000000000, 0.000000000000000000, 0.000000000000000000 ) ) ;
#1918 = EDGE_CURVE ( 'NONE', #7228, #1776, #7775, .T. ) ;
#1919 = ORIENTED_EDGE ( 'NONE', *, *, #1466, .F. ) ;
#1920 = CARTESIAN_POINT ( 'NONE',  ( -4.000000000000000000, 2.309401076758496263, -0.3572655899081631503 ) ) ;
#1921 = CARTESIAN_POINT ( 'NONE',  ( 24.00000000000000000, 1.971681346627238735E-16, -1.610000000000000098 ) ) ;
#1922 = DIRECTION ( 'NONE',  ( 0.000000000000000000, 0.000000000000000000, -1.000000000000000000 ) ) ;
#1923 =( GEOMETRIC_REPRESENTATION_CONTEXT ( 3 ) GLOBAL_UNCERTAINTY_ASSIGNED_CONTEXT ( ( #7447 ) ) GLOBAL_UNIT_ASSIGNED_CONTEXT ( ( #6567, #2842, #3508 ) ) REPRESENTATION_CONTEXT ( 'NONE', 'WORKASPACE' ) );
#1924 = EDGE_CURVE ( 'NONE', #6853, #953, #3157, .T. ) ;
#1925 = FACE_OUTER_BOUND ( 'NONE', #6276, .T. ) ;
#1926 = CARTESIAN_POINT ( 'NONE',  ( 50.00000000000004974, 85.31712395750716382, -2.400000000000014566 ) ) ;
#1927 = ORIENTED_EDGE ( 'NONE', *, *, #6539, .T. ) ;
#1928 = AXIS2_PLACEMENT_3D ( 'NONE', #6859, #3715, #3089 ) ;
#1929 = EDGE_LOOP ( 'NONE', ( #1659, #1013, #4295 ) ) ;
#1930 = CARTESIAN_POINT ( 'NONE',  ( -30.00000000000000355, -29.99999999999999289, 10.00000000000000000 ) ) ;
#1931 = EDGE_LOOP ( 'NONE', ( #7376, #6911 ) ) ;
#1932 = ORIENTED_EDGE ( 'NONE', *, *, #33, .T. ) ;
#1933 = CARTESIAN_POINT ( 'NONE',  ( 60.00000000000000711, 10.00000000000000000, 60.00000000000000000 ) ) ;
#1934 = VECTOR ( 'NONE', #2811, 1000.000000000000000 ) ;
#1935 = CARTESIAN_POINT ( 'NONE',  ( 2.000000000000000000, 0.000000000000000000, 1.535500000000000087 ) ) ;
#1936 = DIRECTION ( 'NONE',  ( -1.000000000000000000, 0.000000000000000000, 0.000000000000000000 ) ) ;
#1937 =( NAMED_UNIT ( * ) SI_UNIT ( $, .STERADIAN. ) SOLID_ANGLE_UNIT ( ) );
#1938 = EDGE_CURVE ( 'NONE', #5254, #604, #6760, .T. ) ;
#1939 = ORIENTED_EDGE ( 'NONE', *, *, #871, .F. ) ;
#1940 = EDGE_CURVE ( 'NONE', #3623, #1156, #4198, .T. ) ;
#1941 = EDGE_LOOP ( 'NONE', ( #6862, #6850 ) ) ;
#1942 = ORIENTED_EDGE ( 'NONE', *, *, #4581, .T. ) ;
#1943 = CYLINDRICAL_SURFACE ( 'NONE', #1586, 1.599999999999992983 ) ;
#1944 = CARTESIAN_POINT ( 'NONE',  ( 42.00000000000003553, 85.00000000000012790, -2.399999999999999023 ) ) ;
#1945 = DIRECTION ( 'NONE',  ( -0.000000000000000000, -0.000000000000000000, 1.000000000000000000 ) ) ;
#1946 = SURFACE_SIDE_STYLE ('',( #6452 ) ) ;
#1947 = ORIENTED_EDGE ( 'NONE', *, *, #3242, .F. ) ;
#1948 = ADVANCED_FACE ( 'NONE', ( #4312, #6308 ), #7555, .F. ) ;
#1949 = CYLINDRICAL_SURFACE ( 'NONE', #7815, 2.149999999999995470 ) ;
#1950 = DIRECTION ( 'NONE',  ( 1.412205397084881070E-17, -2.775557561562891967E-17, -1.000000000000000000 ) ) ;
#1951 = DIRECTION ( 'NONE',  ( 0.000000000000000000, -0.4999999999999992228, 0.8660254037844390407 ) ) ;
#1952 = DIRECTION ( 'NONE',  ( 0.000000000000000000, 0.4999999999999992228, -0.8660254037844390407 ) ) ;
#1953 = ADVANCED_FACE ( 'NONE', ( #478 ), #6050, .F. ) ;
#1954 = CARTESIAN_POINT ( 'NONE',  ( -31.74999999999994316, 0.000000000000000000, 0.000000000000000000 ) ) ;
#1955 = LINE ( 'NONE', #2535, #5535 ) ;
#1956 = VECTOR ( 'NONE', #6675, 1000.000000000000000 ) ;
#1957 = EDGE_CURVE ( 'NONE', #4688, #117, #6136, .T. ) ;
#1958 = ORIENTED_EDGE ( 'NONE', *, *, #6729, .T. ) ;
#1959 = LINE ( 'NONE', #2038, #2174 ) ;
#1960 = APPLICATION_CONTEXT ( 'automotive_design' ) ;
#1961 = CARTESIAN_POINT ( 'NONE',  ( 2.500000000000002220, -1.178949249685215417, 2.042000000000002036 ) ) ;
#1962 = CARTESIAN_POINT ( 'NONE',  ( -4.000000000000000000, 1.935983797701054998, -0.2494693066162268769 ) ) ;
#1963 = CARTESIAN_POINT ( 'NONE',  ( -49.99924596088969508, 84.68545893936895652, 2.384433782424337789 ) ) ;
#1964 = AXIS2_PLACEMENT_3D ( 'NONE', #3827, #6457, #2034 ) ;
#1965 = ORIENTED_EDGE ( 'NONE', *, *, #6264, .F. ) ;
#1966 = VERTEX_POINT ( 'NONE', #4898 ) ;
#1967 = DIRECTION ( 'NONE',  ( 1.000000000000000000, 0.000000000000000000, 0.000000000000000000 ) ) ;
#1968 = ORIENTED_EDGE ( 'NONE', *, *, #7077, .F. ) ;
#1969 = VERTEX_POINT ( 'NONE', #528 ) ;
#1970 = CARTESIAN_POINT ( 'NONE',  ( 0.000000000000000000, 0.000000000000000000, 3.851859888774471706E-31 ) ) ;
#1971 = CARTESIAN_POINT ( 'NONE',  ( 0.000000000000000000, -0.8865213383406685965, 1.535500000000000531 ) ) ;
#1972 = DIRECTION ( 'NONE',  ( 1.000000000000000000, 0.000000000000000000, 0.000000000000000000 ) ) ;
#1973 = DIRECTION ( 'NONE',  ( 0.3194010139189171760, -0.9476196453786549512, 2.921348258588072246E-17 ) ) ;
#1974 = AXIS2_PLACEMENT_3D ( 'NONE', #7930, #6117, #5377 ) ;
#1975 = VERTEX_POINT ( 'NONE', #3071 ) ;
#1976 =( GEOMETRIC_REPRESENTATION_CONTEXT ( 3 ) GLOBAL_UNCERTAINTY_ASSIGNED_CONTEXT ( ( #4873 ) ) GLOBAL_UNIT_ASSIGNED_CONTEXT ( ( #3604, #3010, #4941 ) ) REPRESENTATION_CONTEXT ( 'NONE', 'WORKASPACE' ) );
#1977 = ORIENTED_EDGE ( 'NONE', *, *, #3275, .F. ) ;
#1978 = ORIENTED_EDGE ( 'NONE', *, *, #2262, .T. ) ;
#1979 = FACE_BOUND ( 'NONE', #7402, .T. ) ;
#1980 = ADVANCED_FACE ( 'NONE', ( #2443, #1827 ), #6886, .T. ) ;
#1981 = CARTESIAN_POINT ( 'NONE',  ( 41.93161561614421373, 82.60424888756949713, 0.1913511295313893579 ) ) ;
#1982 = DIRECTION ( 'NONE',  ( 0.000000000000000000, -1.000000000000000000, 0.000000000000000000 ) ) ;
#1983 = EDGE_CURVE ( 'NONE', #4068, #4327, #1200, .T. ) ;
#1984 = VECTOR ( 'NONE', #113, 1000.000000000000000 ) ;
#1985 =( NAMED_UNIT ( * ) SI_UNIT ( $, .STERADIAN. ) SOLID_ANGLE_UNIT ( ) );
#1986 = CARTESIAN_POINT ( 'NONE',  ( -0.9110278382907691652, -6.955741332015764833, 8.000433768563103953 ) ) ;
#1987 = AXIS2_PLACEMENT_3D ( 'NONE', #946, #4279, #1026 ) ;
#1988 = VECTOR ( 'NONE', #4498, 1000.000000000000000 ) ;
#1989 = CIRCLE ( 'NONE', #3035, 1.535500000000000087 ) ;
#1990 = CYLINDRICAL_SURFACE ( 'NONE', #372, 7.000000000000000000 ) ;
#1991 = CARTESIAN_POINT ( 'NONE',  ( 0.000000000000000000, 0.000000000000000000, 18.00000000000000355 ) ) ;
#1992 = CARTESIAN_POINT ( 'NONE',  ( 11.00000000000000355, 0.000000000000000000, 0.000000000000000000 ) ) ;
#1993 = DIRECTION ( 'NONE',  ( 1.000000000000000000, 0.000000000000000000, 0.000000000000000000 ) ) ;
#1994 = AXIS2_PLACEMENT_3D ( 'NONE', #7084, #1364, #5033 ) ;
#1995 = AXIS2_PLACEMENT_3D ( 'NONE', #27, #4943, #6795 ) ;
#1996 = FACE_OUTER_BOUND ( 'NONE', #7227, .T. ) ;
#1997 = CARTESIAN_POINT ( 'NONE',  ( -49.94313152867111683, 87.38422970439138737, -0.3160888171752656572 ) ) ;
#1998 = EDGE_CURVE ( 'NONE', #7134, #931, #5155, .T. ) ;
#1999 = ADVANCED_FACE ( 'NONE', ( #5997, #7749 ), #2614, .F. ) ;
#2000 = CIRCLE ( 'NONE', #4383, 2.649999999999999467 ) ;
#2001 = ORIENTED_EDGE ( 'NONE', *, *, #7821, .F. ) ;
#2002 = AXIS2_PLACEMENT_3D ( 'NONE', #4200, #1762, #6191 ) ;
#2003 = CYLINDRICAL_SURFACE ( 'NONE', #6823, 42.00000000000002132 ) ;
#2004 = CIRCLE ( 'NONE', #5308, 0.1499999999999999667 ) ;
#2005 = CONICAL_SURFACE ( 'NONE', #7034, 1.610000000000000098, 0.7853981633974652654 ) ;
#2006 = PLANE ( 'NONE',  #4510 ) ;
#2007 = CARTESIAN_POINT ( 'NONE',  ( 5.200000000000020606, 0.000000000000000000, -6.938893903907228378E-15 ) ) ;
#2008 = CARTESIAN_POINT ( 'NONE',  ( 24.00000000000000000, 2.210487472460972698E-16, -1.610000000000000098 ) ) ;
#2009 = ORIENTED_EDGE ( 'NONE', *, *, #1846, .T. ) ;
#2010 = AXIS2_PLACEMENT_3D ( 'NONE', #2629, #4499, #3883 ) ;
#2011 = ORIENTED_EDGE ( 'NONE', *, *, #4937, .T. ) ;
#2012 = CARTESIAN_POINT ( 'NONE',  ( -4.000000000000000000, -0.7779732554280796020, -2.666455648918322208 ) ) ;
#2013 = VERTEX_POINT ( 'NONE', #1329 ) ;
#2014 = VERTEX_POINT ( 'NONE', #7638 ) ;
#2015 = CIRCLE ( 'NONE', #1877, 50.00000000000002132 ) ;
#2016 = DIRECTION ( 'NONE',  ( -1.000000000000000000, 0.000000000000000000, 0.000000000000000000 ) ) ;
#2017 = CARTESIAN_POINT ( 'NONE',  ( -38.58716857408418122, 108.0000000000001990, -4.999999999999976907 ) ) ;
#2018 = CARTESIAN_POINT ( 'NONE',  ( 0.000000000000000000, 0.8865213383406723713, 1.535499999999998755 ) ) ;
#2019 =( LENGTH_UNIT ( ) NAMED_UNIT ( * ) SI_UNIT ( .MILLI., .METRE. ) );
#2020 = AXIS2_PLACEMENT_3D ( 'NONE', #1954, #608, #4482 ) ;
#2021 = ORIENTED_EDGE ( 'NONE', *, *, #5845, .F. ) ;
#2022 = ORIENTED_EDGE ( 'NONE', *, *, #3930, .F. ) ;
#2023 = EDGE_CURVE ( 'NONE', #3366, #3705, #1955, .T. ) ;
#2024 = ORIENTED_EDGE ( 'NONE', *, *, #593, .F. ) ;
#2025 = DIRECTION ( 'NONE',  ( 1.412205397084881070E-17, -2.775557561562891967E-17, -1.000000000000000000 ) ) ;
#2026 = CARTESIAN_POINT ( 'NONE',  ( 42.00000000000003553, 85.00000000000012790, -2.399999999999999023 ) ) ;
#2027 = DIRECTION ( 'NONE',  ( -0.000000000000000000, -0.000000000000000000, -1.000000000000000000 ) ) ;
#2028 = CARTESIAN_POINT ( 'NONE',  ( -4.624865572637439470, -5.274399087326279378, 8.014755761910349108 ) ) ;
#2029 = DIRECTION ( 'NONE',  ( -1.000000000000000000, 0.000000000000000000, 0.000000000000000000 ) ) ;
#2030 = CARTESIAN_POINT ( 'NONE',  ( 55.00000000000000000, 10.00000000000000000, 15.50000000000000355 ) ) ;
#2031 = CARTESIAN_POINT ( 'NONE',  ( 20.00000000000000355, 0.000000000000000000, 1.610000000000000098 ) ) ;
#2032 = CARTESIAN_POINT ( 'NONE',  ( 55.00000000000000000, -8.000000000000001776, -6.149999999999981704 ) ) ;
#2033 = ADVANCED_FACE ( 'NONE', ( #7126 ), #7716, .T. ) ;
#2034 = DIRECTION ( 'NONE',  ( 0.000000000000000000, 0.000000000000000000, 1.000000000000000000 ) ) ;
#2035 = AXIS2_PLACEMENT_3D ( 'NONE', #7289, #2763, #7240 ) ;
#2036 = EDGE_CURVE ( 'NONE', #5534, #1891, #762, .T. ) ;
#2037 = ORIENTED_EDGE ( 'NONE', *, *, #6966, .T. ) ;
#2038 = CARTESIAN_POINT ( 'NONE',  ( 52.00000000000000711, 8.000000000000000000, -8.000000000000000000 ) ) ;
#2039 = DIRECTION ( 'NONE',  ( 1.412205397084881070E-17, -2.775557561562891967E-17, -1.000000000000000000 ) ) ;
#2040 = DIRECTION ( 'NONE',  ( -1.000000000000000000, 0.000000000000000000, 0.000000000000000000 ) ) ;
#2041 = CARTESIAN_POINT ( 'NONE',  ( 4.000000000000003553, 0.000000000000000000, 3.500000000000000000 ) ) ;
#2042 = ADVANCED_FACE ( 'NONE', ( #62 ), #5772, .F. ) ;
#2043 = DIRECTION ( 'NONE',  ( -0.000000000000000000, 1.000000000000000000, -0.000000000000000000 ) ) ;
#2044 = ORIENTED_EDGE ( 'NONE', *, *, #7176, .F. ) ;
#2045 = CARTESIAN_POINT ( 'NONE',  ( 49.97873132679187336, 83.53599209938494141, 1.908173386893731616 ) ) ;
#2046 = ORIENTED_EDGE ( 'NONE', *, *, #3723, .F. ) ;
#2047 = CARTESIAN_POINT ( 'NONE',  ( 2.000000000000000000, -1.773042676681340968, 2.059984127722458425E-15 ) ) ;
#2048 = ORIENTED_EDGE ( 'NONE', *, *, #3063, .F. ) ;
#2049 = ORIENTED_EDGE ( 'NONE', *, *, #1688, .F. ) ;
#2050 = CARTESIAN_POINT ( 'NONE',  ( -2.650000000000013678, 3.245314017740498288E-16, 14.60000000000000142 ) ) ;
#2051 = DIRECTION ( 'NONE',  ( 0.000000000000000000, 1.000000000000000000, -0.000000000000000000 ) ) ;
#2052 = DIRECTION ( 'NONE',  ( -0.1425749920180481300, 0.9897840025233048955, -7.267670977394579924E-17 ) ) ;
#2053 =( GEOMETRIC_REPRESENTATION_CONTEXT ( 3 ) GLOBAL_UNCERTAINTY_ASSIGNED_CONTEXT ( ( #2155 ) ) GLOBAL_UNIT_ASSIGNED_CONTEXT ( ( #7816, #5338, #2209 ) ) REPRESENTATION_CONTEXT ( 'NONE', 'WORKASPACE' ) );
#2054 = ORIENTED_EDGE ( 'NONE', *, *, #1506, .T. ) ;
#2055 = ORIENTED_EDGE ( 'NONE', *, *, #1805, .T. ) ;
#2056 = ORIENTED_EDGE ( 'NONE', *, *, #8008, .F. ) ;
#2057 = EDGE_CURVE ( 'NONE', #314, #5998, #7119, .T. ) ;
#2058 = DIRECTION ( 'NONE',  ( 0.000000000000000000, 0.000000000000000000, -1.000000000000000000 ) ) ;
#2059 = CARTESIAN_POINT ( 'NONE',  ( 41.93240078214817146, 87.38208359661221891, 0.3192077737421512018 ) ) ;
#2060 = CARTESIAN_POINT ( 'NONE',  ( 3.099999999999998757, 0.000000000000000000, 0.000000000000000000 ) ) ;
#2061 =( NAMED_UNIT ( * ) SI_UNIT ( $, .STERADIAN. ) SOLID_ANGLE_UNIT ( ) );
#2062 = VECTOR ( 'NONE', #660, 1000.000000000000000 ) ;
#2063 = FACE_BOUND ( 'NONE', #5582, .T. ) ;
#2064 = DIRECTION ( 'NONE',  ( 1.412205397084881070E-17, -2.775557561562891967E-17, -1.000000000000000000 ) ) ;
#2065 = DIRECTION ( 'NONE',  ( 0.000000000000000000, 0.000000000000000000, 1.000000000000000000 ) ) ;
#2066 = PLANE ( 'NONE',  #5073 ) ;
#2067 = DIRECTION ( 'NONE',  ( 0.000000000000000000, -0.4999999999999990563, 0.8660254037844391517 ) ) ;
#2068 = ORIENTED_EDGE ( 'NONE', *, *, #6931, .T. ) ;
#2069 = LINE ( 'NONE', #809, #1934 ) ;
#2070 = EDGE_CURVE ( 'NONE', #4916, #1429, #3080, .T. ) ;
#2071 =( LENGTH_UNIT ( ) NAMED_UNIT ( * ) SI_UNIT ( .MILLI., .METRE. ) );
#2072 = FACE_BOUND ( 'NONE', #6257, .T. ) ;
#2073 = ADVANCED_FACE ( 'NONE', ( #729 ), #3274, .F. ) ;
#2074 = DIRECTION ( 'NONE',  ( -1.000000000000000000, -0.000000000000000000, -0.000000000000000000 ) ) ;
#2075 = EDGE_CURVE ( 'NONE', #855, #1392, #8118, .T. ) ;
#2076 = DIRECTION ( 'NONE',  ( 0.000000000000000000, -0.4999999999999990563, 0.8660254037844391517 ) ) ;
#2077 = EDGE_LOOP ( 'NONE', ( #2293, #8146, #5181, #7575 ) ) ;
#2078 = FACE_OUTER_BOUND ( 'NONE', #5602, .T. ) ;
#2079 = AXIS2_PLACEMENT_3D ( 'NONE', #6156, #3544, #6821 ) ;
#2080 = ORIENTED_EDGE ( 'NONE', *, *, #6628, .T. ) ;
#2081 = ORIENTED_EDGE ( 'NONE', *, *, #4258, .T. ) ;
#2082 = CARTESIAN_POINT ( 'NONE',  ( 1.300000000000000044, -0.7390083445627200209, 1.280000000000001137 ) ) ;
#2083 = AXIS2_PLACEMENT_3D ( 'NONE', #7209, #4180, #7833 ) ;
#2084 = AXIS2_PLACEMENT_3D ( 'NONE', #2485, #2977, #3743 ) ;
#2085 = CARTESIAN_POINT ( 'NONE',  ( 2.099999999999999645, 0.000000000000000000, -0.2800830152838832965 ) ) ;
#2086 = CARTESIAN_POINT ( 'NONE',  ( 50.00000000000000000, -10.00000000000000000, 60.00000000000000000 ) ) ;
#2087 = CONTEXT_DEPENDENT_SHAPE_REPRESENTATION ( #4653, #3799 ) ;
#2088 = EDGE_LOOP ( 'NONE', ( #5858, #38, #365, #740, #1417, #6513 ) ) ;
#2089 = ORIENTED_EDGE ( 'NONE', *, *, #3355, .F. ) ;
#2090 = ORIENTED_EDGE ( 'NONE', *, *, #1631, .T. ) ;
#2091 = CARTESIAN_POINT ( 'NONE',  ( 2.000000000000000000, 1.773042676681340968, -2.276824562219559311E-15 ) ) ;
#2092 = CARTESIAN_POINT ( 'NONE',  ( 4.269299642044305010, -5.566066101761777851, 8.012536085362354399 ) ) ;
#2093 = FACE_OUTER_BOUND ( 'NONE', #5244, .T. ) ;
#2094 = FACE_OUTER_BOUND ( 'NONE', #6279, .T. ) ;
#2095 = EDGE_CURVE ( 'NONE', #2510, #6841, #4753, .T. ) ;
#2096 = EDGE_CURVE ( 'NONE', #550, #2318, #4555, .T. ) ;
#2097 = CIRCLE ( 'NONE', #6736, 3.999999999999999112 ) ;
#2098 = DIRECTION ( 'NONE',  ( 0.000000000000000000, 0.000000000000000000, 1.000000000000000000 ) ) ;
#2099 = CARTESIAN_POINT ( 'NONE',  ( 0.000000000000000000, -0.8865213383406721492, -1.535499999999999199 ) ) ;
#2100 = CARTESIAN_POINT ( 'NONE',  ( 0.000000000000000000, 0.7390083445627193548, -1.280000000000000693 ) ) ;
#2101 = APPLICATION_CONTEXT ( 'automotive_design' ) ;
#2102 = CIRCLE ( 'NONE', #891, 42.00000000000002132 ) ;
#2103 = CARTESIAN_POINT ( 'NONE',  ( -54.99999999999990052, 10.00000000000000000, 15.49999999999877254 ) ) ;
#2104 = CIRCLE ( 'NONE', #6349, 42.00000000000002132 ) ;
#2105 = ADVANCED_FACE ( 'NONE', ( #5384 ), #4132, .F. ) ;
#2106 = ORIENTED_EDGE ( 'NONE', *, *, #7727, .F. ) ;
#2107 = CARTESIAN_POINT ( 'NONE',  ( 1.300000000000000044, 1.478016689125442484, -1.626303258728256651E-15 ) ) ;
#2108 =( LENGTH_UNIT ( ) NAMED_UNIT ( * ) SI_UNIT ( .MILLI., .METRE. ) );
#2109 = DIRECTION ( 'NONE',  ( 0.000000000000000000, 1.000000000000000000, -1.103561164596346103E-15 ) ) ;
#2110 = AXIS2_PLACEMENT_3D ( 'NONE', #6934, #8169, #8134 ) ;
#2111 = AXIS2_PLACEMENT_3D ( 'NONE', #555, #3635, #6698 ) ;
#2112 = DIRECTION ( 'NONE',  ( -1.000000000000000000, -0.000000000000000000, -0.000000000000000000 ) ) ;
#2113 = DIRECTION ( 'NONE',  ( -0.000000000000000000, -0.000000000000000000, 1.000000000000000000 ) ) ;
#2114 = DIRECTION ( 'NONE',  ( 0.000000000000000000, 0.000000000000000000, -1.000000000000000000 ) ) ;
#2115 = VERTEX_POINT ( 'NONE', #180 ) ;
#2116 = CIRCLE ( 'NONE', #4910, 4.999999999999993783 ) ;
#2117 = LINE ( 'NONE', #5245, #3398 ) ;
#2118 = AXIS2_PLACEMENT_3D ( 'NONE', #5795, #6919, #7704 ) ;
#2119 = EDGE_CURVE ( 'NONE', #4877, #5664, #952, .T. ) ;
#2120 = ORIENTED_EDGE ( 'NONE', *, *, #621, .F. ) ;
#2121 = CIRCLE ( 'NONE', #3049, 1.649999999999998579 ) ;
#2122 = VERTEX_POINT ( 'NONE', #5959 ) ;
#2123 = FACE_OUTER_BOUND ( 'NONE', #4286, .T. ) ;
#2124 = FACE_BOUND ( 'NONE', #2902, .T. ) ;
#2125 = DIRECTION ( 'NONE',  ( 0.000000000000000000, 0.000000000000000000, -1.000000000000000000 ) ) ;
#2126 = VECTOR ( 'NONE', #5355, 1000.000000000000000 ) ;
#2127 = ORIENTED_EDGE ( 'NONE', *, *, #5637, .T. ) ;
#2128 = CIRCLE ( 'NONE', #3206, 4.999999999999993783 ) ;
#2129 = VERTEX_POINT ( 'NONE', #6619 ) ;
#2130 = EDGE_LOOP ( 'NONE', ( #2469, #3665, #7353, #7621 ) ) ;
#2131 = CARTESIAN_POINT ( 'NONE',  ( 3.099999999999998757, 0.000000000000000000, 0.000000000000000000 ) ) ;
#2132 = FACE_OUTER_BOUND ( 'NONE', #228, .T. ) ;
#2133 = DIRECTION ( 'NONE',  ( 0.000000000000000000, 0.000000000000000000, 1.000000000000000000 ) ) ;
#2134 = STYLED_ITEM ( 'NONE', ( #1734 ), #1247 ) ;
#2135 = ADVANCED_FACE ( 'NONE', ( #2142, #1484 ), #6036, .F. ) ;
#2136 = EDGE_CURVE ( 'NONE', #4874, #1609, #5617, .T. ) ;
#2137 = EDGE_CURVE ( 'NONE', #6584, #6037, #1607, .T. ) ;
#2138 = CARTESIAN_POINT ( 'NONE',  ( 2.000000000000027089, 3.464101615137739731, -2.700000000000001066 ) ) ;
#2139 = DIRECTION ( 'NONE',  ( -1.000000000000000000, 0.000000000000000000, 0.000000000000000000 ) ) ;
#2140 = SURFACE_STYLE_USAGE ( .BOTH. , #6033 ) ;
#2141 = FACE_BOUND ( 'NONE', #3104, .T. ) ;
#2142 = FACE_BOUND ( 'NONE', #8138, .T. ) ;
#2143 = ORIENTED_EDGE ( 'NONE', *, *, #197, .F. ) ;
#2144 = DIRECTION ( 'NONE',  ( -1.000000000000000000, -0.000000000000000000, -0.000000000000000000 ) ) ;
#2145 = DIRECTION ( 'NONE',  ( 0.000000000000000000, 0.000000000000000000, -1.000000000000000000 ) ) ;
#2146 = LINE ( 'NONE', #5964, #355 ) ;
#2147 = LINE ( 'NONE', #3330, #2755 ) ;
#2148 = DIRECTION ( 'NONE',  ( -1.000000000000000000, 0.000000000000000000, 0.000000000000000000 ) ) ;
#2149 = CARTESIAN_POINT ( 'NONE',  ( -49.95667649488481032, 82.91716997302802383, 1.202799388691194959 ) ) ;
#2150 = VECTOR ( 'NONE', #7177, 1000.000000000000000 ) ;
#2151 = ADVANCED_FACE ( 'NONE', ( #1011 ), #5884, .F. ) ;
#2152 = DIRECTION ( 'NONE',  ( 1.000000000000000000, 0.000000000000000000, -0.000000000000000000 ) ) ;
#2153 = ORIENTED_EDGE ( 'NONE', *, *, #6516, .F. ) ;
#2154 = CARTESIAN_POINT ( 'NONE',  ( 2.000000000000000000, -0.8865213383406690406, 1.535500000000000975 ) ) ;
#2155 = UNCERTAINTY_MEASURE_WITH_UNIT (LENGTH_MEASURE( 1.000000000000000082E-05 ), #7816, 'distance_accuracy_value', 'NONE');
#2156 = EDGE_LOOP ( 'NONE', ( #6877, #955, #1394, #7063 ) ) ;
#2157 = ORIENTED_EDGE ( 'NONE', *, *, #8069, .F. ) ;
#2158 = CYLINDRICAL_SURFACE ( 'NONE', #5564, 2.750000000000000000 ) ;
#2159 = DIRECTION ( 'NONE',  ( -0.000000000000000000, -0.000000000000000000, 1.000000000000000000 ) ) ;
#2160 = CARTESIAN_POINT ( 'NONE',  ( 19.61000000000001720, 0.000000000000000000, 2.000000000000000888 ) ) ;
#2161 = DIRECTION ( 'NONE',  ( 0.000000000000000000, -1.000000000000000000, 0.000000000000000000 ) ) ;
#2162 = ITEM_DEFINED_TRANSFORMATION ( 'NONE', 'NONE', #5118,  #1587 ) ;
#2163 = ORIENTED_EDGE ( 'NONE', *, *, #6444, .F. ) ;
#2164 = VERTEX_POINT ( 'NONE', #337 ) ;
#2165 = ORIENTED_EDGE ( 'NONE', *, *, #4599, .T. ) ;
#2166 = DIRECTION ( 'NONE',  ( -0.000000000000000000, -0.000000000000000000, 1.000000000000000000 ) ) ;
#2167 = EDGE_CURVE ( 'NONE', #6726, #4663, #5600, .T. ) ;
#2168 = CARTESIAN_POINT ( 'NONE',  ( 3.700545867704406966, -5.946256225702112097, 8.009468413176323409 ) ) ;
#2169 = CARTESIAN_POINT ( 'NONE',  ( 3.999999999999989786, -2.309401076758547777, -0.3572655899081733644 ) ) ;
#2170 =( GEOMETRIC_REPRESENTATION_CONTEXT ( 3 ) GLOBAL_UNCERTAINTY_ASSIGNED_CONTEXT ( ( #2378 ) ) GLOBAL_UNIT_ASSIGNED_CONTEXT ( ( #4089, #7825, #1516 ) ) REPRESENTATION_CONTEXT ( 'NONE', 'WORKASPACE' ) );
#2171 = EDGE_CURVE ( 'NONE', #8104, #6902, #7460, .T. ) ;
#2172 = CARTESIAN_POINT ( 'NONE',  ( 27.34999999999998010, 30.00000000000001421, 4.599999999999997868 ) ) ;
#2173 = LINE ( 'NONE', #4130, #7287 ) ;
#2174 = VECTOR ( 'NONE', #5693, 1000.000000000000000 ) ;
#2175 = CARTESIAN_POINT ( 'NONE',  ( 0.000000000000000000, 0.000000000000000000, 18.00000000000000355 ) ) ;
#2176 = CARTESIAN_POINT ( 'NONE',  ( 0.6543461111163455524, 4.241015250120812929, -2.560849780464856895 ) ) ;
#2177 = B_SPLINE_CURVE_WITH_KNOTS ( 'NONE', 3,
 ( #7383, #5525, #1701, #4234, #3655, #444 ),
 .UNSPECIFIED., .F., .F.,
 ( 4, 2, 4 ),
 ( 0.002336974151641521731, 0.003500975885716454527, 0.004664977619791387323 ),
 .UNSPECIFIED. ) ;
#2178 = EDGE_CURVE ( 'NONE', #7471, #1461, #4094, .T. ) ;
#2179 = ORIENTED_EDGE ( 'NONE', *, *, #2648, .T. ) ;
#2180 = ORIENTED_EDGE ( 'NONE', *, *, #5385, .T. ) ;
#2181 = CARTESIAN_POINT ( 'NONE',  ( 57.99999999999999289, -8.000000000000003553, 11.99999999999998934 ) ) ;
#2182 = EDGE_CURVE ( 'NONE', #4855, #2250, #5918, .T. ) ;
#2183 = CARTESIAN_POINT ( 'NONE',  ( 3.673643420401898840, 2.497823135841254150, -2.451519936625006668 ) ) ;
#2184 = CARTESIAN_POINT ( 'NONE',  ( -7.000000000000000000, 0.000000000000000000, 0.000000000000000000 ) ) ;
#2185 = CYLINDRICAL_SURFACE ( 'NONE', #6874, 1.599999999999992983 ) ;
#2186 = CARTESIAN_POINT ( 'NONE',  ( -30.00000000000000355, -29.99999999999999289, 10.00000000000000000 ) ) ;
#2187 = DIRECTION ( 'NONE',  ( 1.000000000000000000, 0.000000000000000000, 0.000000000000000000 ) ) ;
#2188 = CARTESIAN_POINT ( 'NONE',  ( 1.274374112546295138E-14, 85.00000000000017053, 2.000000000000043521 ) ) ;
#2189 =( REPRESENTATION_RELATIONSHIP ('NONE','NONE', #3916, #2201 ) REPRESENTATION_RELATIONSHIP_WITH_TRANSFORMATION ( #6183 )SHAPE_REPRESENTATION_RELATIONSHIP( ) );
#2190 = ORIENTED_EDGE ( 'NONE', *, *, #945, .T. ) ;
#2191 = CARTESIAN_POINT ( 'NONE',  ( 55.00000000000000000, 10.00000000000000000, -4.499999999999986677 ) ) ;
#2192 = EDGE_CURVE ( 'NONE', #4327, #6012, #4142, .T. ) ;
#2193 = ORIENTED_EDGE ( 'NONE', *, *, #3938, .T. ) ;
#2194 = ORIENTED_EDGE ( 'NONE', *, *, #3750, .F. ) ;
#2195 = CYLINDRICAL_SURFACE ( 'NONE', #5562, 4.999999999999997335 ) ;
#2196 = CARTESIAN_POINT ( 'NONE',  ( 2.500000000000002220, -1.178949249685215417, 2.042000000000002036 ) ) ;
#2197 = CARTESIAN_POINT ( 'NONE',  ( 50.00000000000000000, 10.00000000000000000, 60.00000000000000000 ) ) ;
#2198 = DIRECTION ( 'NONE',  ( 1.000000000000000000, 0.000000000000000000, 0.000000000000000000 ) ) ;
#2199 = LINE ( 'NONE', #7350, #2221 ) ;
#2200 = CONTEXT_DEPENDENT_SHAPE_REPRESENTATION ( #1798, #2536 ) ;
#2201 = SHAPE_REPRESENTATION ( 'socket head cap screw_iso_ISO 4762 M4 x 16 - 16N', ( #1587 ), #3250 ) ;
#2202 = VERTEX_POINT ( 'NONE', #2215 ) ;
#2203 = ORIENTED_EDGE ( 'NONE', *, *, #6591, .F. ) ;
#2204 = VECTOR ( 'NONE', #7910, 1000.000000000000000 ) ;
#2205 = VERTEX_POINT ( 'NONE', #7898 ) ;
#2206 = CARTESIAN_POINT ( 'NONE',  ( -39.83716857408418122, 108.0000000000001990, -4.999999999999976907 ) ) ;
#2207 = CARTESIAN_POINT ( 'NONE',  ( 0.9200942725349188223, -6.954338967362795110, 8.000447262915827196 ) ) ;
#2208 = LINE ( 'NONE', #4872, #4781 ) ;
#2209 =( NAMED_UNIT ( * ) SI_UNIT ( $, .STERADIAN. ) SOLID_ANGLE_UNIT ( ) );
#2210 = DIRECTION ( 'NONE',  ( -0.000000000000000000, -0.000000000000000000, 1.000000000000000000 ) ) ;
#2211 = EDGE_CURVE ( 'NONE', #5370, #4900, #6485, .T. ) ;
#2212 = DIRECTION ( 'NONE',  ( 1.734723475976806848E-16, -1.000000000000000000, 0.000000000000000000 ) ) ;
#2213 = FACE_OUTER_BOUND ( 'NONE', #6917, .T. ) ;
#2214 = CARTESIAN_POINT ( 'NONE',  ( -1.318516776095820964, -3.857556137907092175, -1.717345860808523723E-14 ) ) ;
#2215 = CARTESIAN_POINT ( 'NONE',  ( 2.000000000000000000, -1.773042676681340524, 1.734723475976807094E-15 ) ) ;
#2216 = AXIS2_PLACEMENT_3D ( 'NONE', #5293, #5987, #4624 ) ;
#2217 = PRESENTATION_LAYER_ASSIGNMENT (  '', '', ( #1437 ) ) ;
#2218 = ORIENTED_EDGE ( 'NONE', *, *, #7389, .F. ) ;
#2219 = ORIENTED_EDGE ( 'NONE', *, *, #2839, .F. ) ;
#2220 = DIRECTION ( 'NONE',  ( 0.000000000000000000, -0.5000000000000013323, -0.8660254037844378194 ) ) ;
#2221 = VECTOR ( 'NONE', #6724, 1000.000000000000000 ) ;
#2222 = CARTESIAN_POINT ( 'NONE',  ( 0.000000000000000000, 0.000000000000000000, 3.299999999999999822 ) ) ;
#2223 = DIRECTION ( 'NONE',  ( 0.000000000000000000, 0.000000000000000000, 1.000000000000000000 ) ) ;
#2224 = CARTESIAN_POINT ( 'NONE',  ( -1.198153218366585720E-14, 42.68016229225776925, 4.000000000000000000 ) ) ;
#2225 = CARTESIAN_POINT ( 'NONE',  ( -34.99999999999999289, -29.99999999999999289, 10.00000000000000000 ) ) ;
#2226 = CARTESIAN_POINT ( 'NONE',  ( -49.97498335796541369, 83.41456698278581428, -1.808729786019619423 ) ) ;
#2227 = AXIS2_PLACEMENT_3D ( 'NONE', #2771, #1490, #7834 ) ;
#2228 = AXIS2_PLACEMENT_3D ( 'NONE', #487, #5406, #2984 ) ;
#2229 = FACE_OUTER_BOUND ( 'NONE', #76, .T. ) ;
#2230 = ADVANCED_FACE ( 'NONE', ( #5552 ), #1185, .F. ) ;
#2231 = ORIENTED_EDGE ( 'NONE', *, *, #5399, .T. ) ;
#2232 = ADVANCED_FACE ( 'NONE', ( #4841, #3678, #1057, #8026 ), #3735, .F. ) ;
#2233 = DIRECTION ( 'NONE',  ( -0.5000000000000024425, 0.8660254037844373753, 0.000000000000000000 ) ) ;
#2234 = EDGE_CURVE ( 'NONE', #2468, #1975, #4424, .T. ) ;
#2235 = ORIENTED_EDGE ( 'NONE', *, *, #2412, .F. ) ;
#2236 = AXIS2_PLACEMENT_3D ( 'NONE', #3540, #4202, #6778 ) ;
#2237 = ORIENTED_EDGE ( 'NONE', *, *, #5989, .T. ) ;
#2238 = CIRCLE ( 'NONE', #4505, 3.500000000000000000 ) ;
#2239 = VECTOR ( 'NONE', #7777, 1000.000000000000000 ) ;
#2240 = DIRECTION ( 'NONE',  ( -1.000000000000000000, -0.000000000000000000, -0.000000000000000000 ) ) ;
#2241 = AXIS2_PLACEMENT_3D ( 'NONE', #4060, #889, #3559 ) ;
#2242 = CARTESIAN_POINT ( 'NONE',  ( -41.08716857408418122, 108.0000000000001990, -4.999999999999976907 ) ) ;
#2243 = CIRCLE ( 'NONE', #6885, 0.2500000000000002220 ) ;
#2244 = DIRECTION ( 'NONE',  ( 0.000000000000000000, 0.000000000000000000, 1.000000000000000000 ) ) ;
#2245 = DIRECTION ( 'NONE',  ( -0.000000000000000000, -0.000000000000000000, 1.000000000000000000 ) ) ;
#2246 = PRODUCT_CONTEXT ( 'NONE', #7736, 'mechanical' ) ;
#2247 = VECTOR ( 'NONE', #7078, 1000.000000000000114 ) ;
#2248 = ORIENTED_EDGE ( 'NONE', *, *, #5800, .T. ) ;
#2249 = AXIS2_PLACEMENT_3D ( 'NONE', #7649, #739, #2499 ) ;
#2250 = VERTEX_POINT ( 'NONE', #7500 ) ;
#2251 = ORIENTED_EDGE ( 'NONE', *, *, #4713, .F. ) ;
#2252 = VECTOR ( 'NONE', #3038, 1000.000000000000000 ) ;
#2253 = CARTESIAN_POINT ( 'NONE',  ( -39.99999999999999289, 40.00000000000000711, 10.00000000000000000 ) ) ;
#2254 = DIRECTION ( 'NONE',  ( 0.000000000000000000, -1.224646799147353207E-16, 1.000000000000000000 ) ) ;
#2255 = AXIS2_PLACEMENT_3D ( 'NONE', #4020, #255, #6032 ) ;
#2256 = AXIS2_PLACEMENT_3D ( 'NONE', #6263, #4271, #7506 ) ;
#2257 = FACE_OUTER_BOUND ( 'NONE', #4121, .T. ) ;
#2258 = VERTEX_POINT ( 'NONE', #6922 ) ;
#2259 = ADVANCED_FACE ( 'NONE', ( #6256 ), #1736, .F. ) ;
#2260 = DIRECTION ( 'NONE',  ( -1.000000000000000000, 0.000000000000000000, 0.000000000000000000 ) ) ;
#2261 = VECTOR ( 'NONE', #5136, 1000.000000000000000 ) ;
#2262 = EDGE_CURVE ( 'NONE', #4453, #7189, #2968, .T. ) ;
#2263 = FACE_OUTER_BOUND ( 'NONE', #441, .T. ) ;
#2264 = CARTESIAN_POINT ( 'NONE',  ( 0.000000000000000000, -0.8865213383406685965, 1.535500000000000531 ) ) ;
#2265 = CARTESIAN_POINT ( 'NONE',  ( -7.000000000000000000, 1.843750452292770530E-16, 8.033969604113661234 ) ) ;
#2266 = CARTESIAN_POINT ( 'NONE',  ( 6.955677005507068245, 0.9111895000360680230, 8.033535213607201797 ) ) ;
#2267 = ORIENTED_EDGE ( 'NONE', *, *, #2993, .T. ) ;
#2268 = ORIENTED_EDGE ( 'NONE', *, *, #4064, .T. ) ;
#2269 = FACE_OUTER_BOUND ( 'NONE', #7338, .T. ) ;
#2270 = CARTESIAN_POINT ( 'NONE',  ( 0.000000000000000000, 0.000000000000000000, -2.700000000000001066 ) ) ;
#2271 = FACE_OUTER_BOUND ( 'NONE', #2307, .T. ) ;
#2272 = FACE_OUTER_BOUND ( 'NONE', #2603, .T. ) ;
#2273 = LINE ( 'NONE', #6711, #6943 ) ;
#2274 = ADVANCED_FACE ( 'NONE', ( #4215 ), #3058, .F. ) ;
#2275 = CARTESIAN_POINT ( 'NONE',  ( 30.00000000000001066, -29.99999999999997868, 10.00000000000000000 ) ) ;
#2276 = ADVANCED_FACE ( 'NONE', ( #5474 ), #3601, .T. ) ;
#2277 = DIRECTION ( 'NONE',  ( -1.000000000000000000, -0.000000000000000000, -0.000000000000000000 ) ) ;
#2278 = ORIENTED_EDGE ( 'NONE', *, *, #3292, .T. ) ;
#2279 = CARTESIAN_POINT ( 'NONE',  ( 57.99999999999999289, 7.999999999999996447, 19.99999999999998934 ) ) ;
#2280 = ORIENTED_EDGE ( 'NONE', *, *, #5761, .T. ) ;
#2281 = ORIENTED_EDGE ( 'NONE', *, *, #4024, .T. ) ;
#2282 = DIRECTION ( 'NONE',  ( 0.000000000000000000, 0.000000000000000000, -1.000000000000000000 ) ) ;
#2283 = PRODUCT_DEFINITION ( 'UNKNOWN', '', #4572, #2500 ) ;
#2284 = CARTESIAN_POINT ( 'NONE',  ( 55.00000000000000000, 10.00000000000000000, 15.50000000000000355 ) ) ;
#2285 = FACE_OUTER_BOUND ( 'NONE', #4077, .T. ) ;
#2286 = CIRCLE ( 'NONE', #3619, 3.999999999999999112 ) ;
#2287 = CARTESIAN_POINT ( 'NONE',  ( -5.271309882437016370, 4.628374325350936402, 8.019190801808186109 ) ) ;
#2288 = DIRECTION ( 'NONE',  ( 0.000000000000000000, 0.000000000000000000, -1.000000000000000000 ) ) ;
#2289 = ITEM_DEFINED_TRANSFORMATION ( 'NONE', 'NONE', #5770,  #1587 ) ;
#2290 = AXIS2_PLACEMENT_3D ( 'NONE', #7413, #5016, #385 ) ;
#2291 = VERTEX_POINT ( 'NONE', #7366 ) ;
#2292 = ORIENTED_EDGE ( 'NONE', *, *, #434, .F. ) ;
#2293 = ORIENTED_EDGE ( 'NONE', *, *, #3907, .F. ) ;
#2294 = B_SPLINE_CURVE_WITH_KNOTS ( 'NONE', 3,
 ( #1741, #3681, #4399, #5684, #8201, #2528 ),
 .UNSPECIFIED., .F., .F.,
 ( 4, 2, 4 ),
 ( 0.004120275011746849653, 0.005288420935197133549, 0.006456566858647417445 ),
 .UNSPECIFIED. ) ;
#2295 = LINE ( 'NONE', #2253, #7936 ) ;
#2296 = PLANE ( 'NONE',  #7161 ) ;
#2297 = FACE_BOUND ( 'NONE', #6331, .T. ) ;
#2298 = ORIENTED_EDGE ( 'NONE', *, *, #7692, .T. ) ;
#2299 = LINE ( 'NONE', #6071, #2615 ) ;
#2300 = EDGE_LOOP ( 'NONE', ( #4111, #3062, #1886, #6280 ) ) ;
#2301 = EDGE_CURVE ( 'NONE', #3918, #2562, #6164, .T. ) ;
#2302 = CARTESIAN_POINT ( 'NONE',  ( 41.97904239022138029, 86.32664991614251448, 2.000000000000043521 ) ) ;
#2303 = CARTESIAN_POINT ( 'NONE',  ( -42.00000000000001421, 84.74546678807557498, -2.399999999999965272 ) ) ;
#2304 =( LENGTH_UNIT ( ) NAMED_UNIT ( * ) SI_UNIT ( .MILLI., .METRE. ) );
#2305 =( GEOMETRIC_REPRESENTATION_CONTEXT ( 3 ) GLOBAL_UNCERTAINTY_ASSIGNED_CONTEXT ( ( #6548 ) ) GLOBAL_UNIT_ASSIGNED_CONTEXT ( ( #2424, #4965, #3133 ) ) REPRESENTATION_CONTEXT ( 'NONE', 'WORKASPACE' ) );
#2306 = DIRECTION ( 'NONE',  ( -1.000000000000000000, -0.000000000000000000, -0.000000000000000000 ) ) ;
#2307 = EDGE_LOOP ( 'NONE', ( #1787, #1932, #6522, #2866, #7072 ) ) ;
#2308 = EDGE_LOOP ( 'NONE', ( #1818, #5430, #1801, #6222, #3675, #134, #6812, #7886 ) ) ;
#2309 = CARTESIAN_POINT ( 'NONE',  ( 29.55500000000002458, 0.000000000000000000, 2.499999999999987121 ) ) ;
#2310 = DIRECTION ( 'NONE',  ( -1.000000000000000000, -0.000000000000000000, -0.000000000000000000 ) ) ;
#2311 = CARTESIAN_POINT ( 'NONE',  ( -42.00000000000000711, 85.00000000000011369, -2.399999999999999911 ) ) ;
#2312 = DIRECTION ( 'NONE',  ( 0.000000000000000000, 0.000000000000000000, 1.000000000000000000 ) ) ;
#2313 = CARTESIAN_POINT ( 'NONE',  ( 20.00000000000000355, 0.000000000000000000, 0.000000000000000000 ) ) ;
#2314 = DIRECTION ( 'NONE',  ( -0.000000000000000000, -0.000000000000000000, 1.000000000000000000 ) ) ;
#2315 = ORIENTED_EDGE ( 'NONE', *, *, #1097, .T. ) ;
#2316 = DIRECTION ( 'NONE',  ( 1.000000000000000000, 0.000000000000000000, 0.000000000000000000 ) ) ;
#2317 = PRODUCT ( 'base', 'base', '', ( #1538 ) ) ;
#2318 = VERTEX_POINT ( 'NONE', #4936 ) ;
#2319 = EDGE_CURVE ( 'NONE', #7228, #1171, #1233, .T. ) ;
#2320 = VERTEX_POINT ( 'NONE', #4977 ) ;
#2321 = ADVANCED_FACE ( 'NONE', ( #5072 ), #8196, .T. ) ;
#2322 = DIRECTION ( 'NONE',  ( 0.000000000000000000, 0.000000000000000000, -1.000000000000000000 ) ) ;
#2323 = EDGE_CURVE ( 'NONE', #3305, #3366, #1908, .T. ) ;
#2324 = CARTESIAN_POINT ( 'NONE',  ( -4.999999999999997335, 6.123233995736758394E-16, 20.00000000000000355 ) ) ;
#2325 = DIRECTION ( 'NONE',  ( -0.000000000000000000, -0.000000000000000000, 1.000000000000000000 ) ) ;
#2326 = CARTESIAN_POINT ( 'NONE',  ( 30.00000000000000000, 2.789133085058097101E-16, -2.055000000000006821 ) ) ;
#2327 = ORIENTED_EDGE ( 'NONE', *, *, #6061, .T. ) ;
#2328 = ORIENTED_EDGE ( 'NONE', *, *, #3057, .F. ) ;
#2329 = ORIENTED_EDGE ( 'NONE', *, *, #5553, .T. ) ;
#2330 = FACE_OUTER_BOUND ( 'NONE', #6430, .T. ) ;
#2331 = FACE_OUTER_BOUND ( 'NONE', #5180, .T. ) ;
#2332 = DIRECTION ( 'NONE',  ( -0.000000000000000000, -0.000000000000000000, 1.000000000000000000 ) ) ;
#2333 = ORIENTED_EDGE ( 'NONE', *, *, #3443, .T. ) ;
#2334 = DIRECTION ( 'NONE',  ( 1.412205397084881070E-17, -2.775557561562891967E-17, -1.000000000000000000 ) ) ;
#2335 = AXIS2_PLACEMENT_3D ( 'NONE', #270, #7961, #4065 ) ;
#2336 = EDGE_LOOP ( 'NONE', ( #1890, #3265 ) ) ;
#2337 = ORIENTED_EDGE ( 'NONE', *, *, #3674, .F. ) ;
#2338 = CARTESIAN_POINT ( 'NONE',  ( 2.500000000000002220, 0.000000000000000000, 0.000000000000000000 ) ) ;
#2339 = FACE_OUTER_BOUND ( 'NONE', #1123, .T. ) ;
#2340 = AXIS2_PLACEMENT_3D ( 'NONE', #6042, #7904, #1563 ) ;
#2341 = VECTOR ( 'NONE', #3320, 1000.000000000000000 ) ;
#2342 = DIRECTION ( 'NONE',  ( -0.5000000000000051070, 1.060575238724903217E-16, -0.8660254037844355990 ) ) ;
#2343 = CARTESIAN_POINT ( 'NONE',  ( 1.587956359206372792, 6.821324887144850635, 8.001713349940533959 ) ) ;
#2344 = ADVANCED_FACE ( 'NONE', ( #6297, #602 ), #3145, .F. ) ;
#2345 = EDGE_LOOP ( 'NONE', ( #7725, #3083, #465, #2855 ) ) ;
#2346 = ORIENTED_EDGE ( 'NONE', *, *, #2525, .T. ) ;
#2347 =( LENGTH_UNIT ( ) NAMED_UNIT ( * ) SI_UNIT ( .MILLI., .METRE. ) );
#2348 = CARTESIAN_POINT ( 'NONE',  ( -41.95400501379501890, 86.96664633062719929, 1.381527937806870998 ) ) ;
#2349 = DIRECTION ( 'NONE',  ( -1.000000000000000000, -1.502586498047605218E-16, 1.238733049487200360E-17 ) ) ;
#2350 = DIRECTION ( 'NONE',  ( 1.412205397084881070E-17, -2.775557561562891967E-17, -1.000000000000000000 ) ) ;
#2351 = VECTOR ( 'NONE', #1638, 1000.000000000000000 ) ;
#2352 = CARTESIAN_POINT ( 'NONE',  ( -54.99999999999990052, 7.999999999999996447, 15.49999999999877254 ) ) ;
#2353 = DIRECTION ( 'NONE',  ( -0.000000000000000000, 1.000000000000000000, -0.000000000000000000 ) ) ;
#2354 = EDGE_CURVE ( 'NONE', #5401, #2014, #5609, .T. ) ;
#2355 = VERTEX_POINT ( 'NONE', #224 ) ;
#2356 = EDGE_LOOP ( 'NONE', ( #7360, #5590, #430, #4551 ) ) ;
#2357 = DIRECTION ( 'NONE',  ( 0.000000000000000000, 0.000000000000000000, 1.000000000000000000 ) ) ;
#2358 = CARTESIAN_POINT ( 'NONE',  ( -31.74999999999995737, 0.000000000000000000, 0.000000000000000000 ) ) ;
#2359 = DIRECTION ( 'NONE',  ( 0.000000000000000000, 0.000000000000000000, 1.000000000000000000 ) ) ;
#2360 = PLANE ( 'NONE',  #6129 ) ;
#2361 = VECTOR ( 'NONE', #7420, 1000.000000000000000 ) ;
#2362 = LINE ( 'NONE', #3529, #7673 ) ;
#2363 = CARTESIAN_POINT ( 'NONE',  ( -42.00000000000000711, 85.00000000000011369, -5.000000000000005329 ) ) ;
#2364 = ITEM_DEFINED_TRANSFORMATION ( 'NONE', 'NONE', #976,  #1587 ) ;
#2365 = ADVANCED_FACE ( 'NONE', ( #2229 ), #2728, .T. ) ;
#2366 = CIRCLE ( 'NONE', #2901, 2.149999999999999023 ) ;
#2367 = APPLICATION_CONTEXT ( 'automotive_design' ) ;
#2368 = VECTOR ( 'NONE', #2240, 1000.000000000000000 ) ;
#2369 = VECTOR ( 'NONE', #6804, 1000.000000000000000 ) ;
#2370 = CIRCLE ( 'NONE', #646, 0.2000000000000000944 ) ;
#2371 = ORIENTED_EDGE ( 'NONE', *, *, #4695, .T. ) ;
#2372 = ORIENTED_EDGE ( 'NONE', *, *, #6735, .F. ) ;
#2373 = ORIENTED_EDGE ( 'NONE', *, *, #5785, .T. ) ;
#2374 = DIRECTION ( 'NONE',  ( 0.000000000000000000, -0.4999999999999990563, 0.8660254037844391517 ) ) ;
#2375 = DIRECTION ( 'NONE',  ( 0.000000000000000000, 0.000000000000000000, 1.000000000000000000 ) ) ;
#2376 = PLANE ( 'NONE',  #93 ) ;
#2377 = MECHANICAL_DESIGN_GEOMETRIC_PRESENTATION_REPRESENTATION (  '', ( #1324 ), #3852 ) ;
#2378 = UNCERTAINTY_MEASURE_WITH_UNIT (LENGTH_MEASURE( 1.000000000000000082E-05 ), #4089, 'distance_accuracy_value', 'NONE');
#2379 = AXIS2_PLACEMENT_3D ( 'NONE', #6250, #4972, #2926 ) ;
#2380 = VECTOR ( 'NONE', #2938, 1000.000000000000000 ) ;
#2381 = EDGE_LOOP ( 'NONE', ( #3082, #5166, #7491 ) ) ;
#2382 = DIRECTION ( 'NONE',  ( 0.000000000000000000, 0.000000000000000000, -1.000000000000000000 ) ) ;
#2383 = AXIS2_PLACEMENT_3D ( 'NONE', #1746, #6884, #1067 ) ;
#2384 = ORIENTED_EDGE ( 'NONE', *, *, #7020, .T. ) ;
#2385 = EDGE_LOOP ( 'NONE', ( #6365, #764, #4734, #7342 ) ) ;
#2386 = CIRCLE ( 'NONE', #377, 1.250000000000001110 ) ;
#2387 = TOROIDAL_SURFACE ( 'NONE', #2783, 2.200000000000001066, 0.2000000000000000111 ) ;
#2388 = DIRECTION ( 'NONE',  ( 0.000000000000000000, 0.000000000000000000, 1.000000000000000000 ) ) ;
#2389 = ADVANCED_FACE ( 'NONE', ( #3444 ), #7320, .F. ) ;
#2390 = CARTESIAN_POINT ( 'NONE',  ( 58.00000000000000000, -8.000000000000000000, -8.000000000000000000 ) ) ;
#2391 = EDGE_CURVE ( 'NONE', #5793, #5534, #980, .T. ) ;
#2392 = FACE_OUTER_BOUND ( 'NONE', #6196, .T. ) ;
#2393 = AXIS2_PLACEMENT_3D ( 'NONE', #7889, #4080, #5336 ) ;
#2394 = DIRECTION ( 'NONE',  ( -1.000000000000000000, -0.000000000000000000, -0.000000000000000000 ) ) ;
#2395 = ORIENTED_EDGE ( 'NONE', *, *, #7434, .T. ) ;
#2396 = AXIS2_PLACEMENT_3D ( 'NONE', #2569, #5111, #1864 ) ;
#2397 = VERTEX_POINT ( 'NONE', #268 ) ;
#2398 = SURFACE_SIDE_STYLE ('',( #7597 ) ) ;
#2399 = LINE ( 'NONE', #4439, #6479 ) ;
#2400 = DIRECTION ( 'NONE',  ( 0.000000000000000000, 0.000000000000000000, 1.000000000000000000 ) ) ;
#2401 = DIRECTION ( 'NONE',  ( 0.000000000000000000, 0.000000000000000000, 1.000000000000000000 ) ) ;
#2402 = CIRCLE ( 'NONE', #800, 2.200000000000001066 ) ;
#2403 = DIRECTION ( 'NONE',  ( -0.000000000000000000, -0.000000000000000000, 1.000000000000000000 ) ) ;
#2404 = PLANE ( 'NONE',  #206 ) ;
#2405 = VERTEX_POINT ( 'NONE', #7302 ) ;
#2406 = ADVANCED_FACE ( 'NONE', ( #1570 ), #3521, .T. ) ;
#2407 = VERTEX_POINT ( 'NONE', #5395 ) ;
#2408 = CARTESIAN_POINT ( 'NONE',  ( -27.35000000000000142, -29.99999999999999289, 4.599999999999997868 ) ) ;
#2409 = LINE ( 'NONE', #3694, #3437 ) ;
#2410 = CARTESIAN_POINT ( 'NONE',  ( 30.00000000000001066, -29.99999999999997868, 4.599999999999997868 ) ) ;
#2411 = CARTESIAN_POINT ( 'NONE',  ( 4.000000000000003553, 2.309401076758524685, -0.3572655899081733644 ) ) ;
#2412 = EDGE_CURVE ( 'NONE', #2593, #6876, #156, .T. ) ;
#2413 = ADVANCED_FACE ( 'NONE', ( #5276 ), #7337, .T. ) ;
#2414 = DIRECTION ( 'NONE',  ( 1.000000000000000000, -0.000000000000000000, -0.000000000000000000 ) ) ;
#2415 = LINE ( 'NONE', #5089, #5290 ) ;
#2416 = ORIENTED_EDGE ( 'NONE', *, *, #6836, .T. ) ;
#2417 = EDGE_LOOP ( 'NONE', ( #284, #4162 ) ) ;
#2418 = VERTEX_POINT ( 'NONE', #5892 ) ;
#2419 = AXIS2_PLACEMENT_3D ( 'NONE', #6581, #4105, #2114 ) ;
#2420 = VERTEX_POINT ( 'NONE', #6046 ) ;
#2421 = CARTESIAN_POINT ( 'NONE',  ( 30.00000000000001066, -29.99999999999997868, 4.599999999999997868 ) ) ;
#2422 = DIRECTION ( 'NONE',  ( -1.000000000000000000, -0.000000000000000000, -0.000000000000000000 ) ) ;
#2423 = CARTESIAN_POINT ( 'NONE',  ( 52.00000000000000711, 8.000000000000000000, -8.000000000000000000 ) ) ;
#2424 =( LENGTH_UNIT ( ) NAMED_UNIT ( * ) SI_UNIT ( .MILLI., .METRE. ) );
#2425 = VECTOR ( 'NONE', #2394, 1000.000000000000000 ) ;
#2426 = EDGE_LOOP ( 'NONE', ( #5090, #7369, #8009, #4999 ) ) ;
#2427 = DIRECTION ( 'NONE',  ( 0.000000000000000000, 0.000000000000000000, -1.000000000000000000 ) ) ;
#2428 = ORIENTED_EDGE ( 'NONE', *, *, #5839, .T. ) ;
#2429 = ORIENTED_EDGE ( 'NONE', *, *, #88, .T. ) ;
#2430 = EDGE_CURVE ( 'NONE', #6596, #4714, #6930, .T. ) ;
#2431 = DIRECTION ( 'NONE',  ( 0.000000000000000000, 0.000000000000000000, 1.000000000000000000 ) ) ;
#2432 = EDGE_CURVE ( 'NONE', #4613, #5533, #1656, .T. ) ;
#2433 = CARTESIAN_POINT ( 'NONE',  ( -41.99757081983619145, 84.48764332354225814, -2.358461006662856185 ) ) ;
#2434 = DIRECTION ( 'NONE',  ( -0.000000000000000000, -0.000000000000000000, 1.000000000000000000 ) ) ;
#2435 = DIRECTION ( 'NONE',  ( 0.000000000000000000, 0.000000000000000000, -1.000000000000000000 ) ) ;
#2436 = ORIENTED_EDGE ( 'NONE', *, *, #4285, .T. ) ;
#2437 = ORIENTED_EDGE ( 'NONE', *, *, #4578, .F. ) ;
#2438 = FACE_BOUND ( 'NONE', #6318, .T. ) ;
#2439 = DIRECTION ( 'NONE',  ( -1.000000000000000000, 0.000000000000000000, 1.412205397084726379E-17 ) ) ;
#2440 = FACE_OUTER_BOUND ( 'NONE', #8159, .T. ) ;
#2441 = PRESENTATION_LAYER_ASSIGNMENT (  '', '', ( #7745 ) ) ;
#2442 = DIRECTION ( 'NONE',  ( 1.000000000000000000, 0.000000000000000000, 0.000000000000000000 ) ) ;
#2443 = FACE_BOUND ( 'NONE', #6635, .T. ) ;
#2444 = EDGE_CURVE ( 'NONE', #2553, #7873, #188, .T. ) ;
#2445 = VERTEX_POINT ( 'NONE', #4767 ) ;
#2446 = EDGE_CURVE ( 'NONE', #6378, #4032, #5359, .T. ) ;
#2447 = ORIENTED_EDGE ( 'NONE', *, *, #5049, .T. ) ;
#2448 = PRODUCT_DEFINITION_FORMATION_WITH_SPECIFIED_SOURCE ( 'ANY', '', #5512, .NOT_KNOWN. ) ;
#2449 = DIRECTION ( 'NONE',  ( -1.000000000000000000, -0.000000000000000000, -0.000000000000000000 ) ) ;
#2450 = FACE_OUTER_BOUND ( 'NONE', #7181, .T. ) ;
#2451 = CARTESIAN_POINT ( 'NONE',  ( 0.000000000000000000, 1.773042676681340968, -2.276824562219559311E-15 ) ) ;
#2452 = DIRECTION ( 'NONE',  ( 1.412205397084881070E-17, -2.775557561562891967E-17, -1.000000000000000000 ) ) ;
#2453 = CARTESIAN_POINT ( 'NONE',  ( 60.00000000000000711, -10.00000000000000000, 0.000000000000000000 ) ) ;
#2454 = CARTESIAN_POINT ( 'NONE',  ( 0.000000000000000000, 2.357898499370434386, -3.469446951953614189E-15 ) ) ;
#2455 = AXIS2_PLACEMENT_3D ( 'NONE', #7243, #2848, #151 ) ;
#2456 = EDGE_LOOP ( 'NONE', ( #1307, #2675 ) ) ;
#2457 = ADVANCED_FACE ( 'NONE', ( #7872, #310 ), #7837, .T. ) ;
#2458 = EDGE_CURVE ( 'NONE', #5123, #1485, #4031, .T. ) ;
#2459 = ORIENTED_EDGE ( 'NONE', *, *, #4862, .T. ) ;
#2460 = ORIENTED_EDGE ( 'NONE', *, *, #784, .T. ) ;
#2461 = VERTEX_POINT ( 'NONE', #2897 ) ;
#2462 = DIRECTION ( 'NONE',  ( 0.000000000000000000, 0.000000000000000000, -1.000000000000000000 ) ) ;
#2463 = FACE_OUTER_BOUND ( 'NONE', #705, .T. ) ;
#2464 = DIRECTION ( 'NONE',  ( 0.000000000000000000, 0.000000000000000000, 1.000000000000000000 ) ) ;
#2465 = SURFACE_SIDE_STYLE ('',( #460 ) ) ;
#2466 = ORIENTED_EDGE ( 'NONE', *, *, #3877, .T. ) ;
#2467 = CARTESIAN_POINT ( 'NONE',  ( 49.95667649488486717, 82.91716997302819436, -1.202799388691395910 ) ) ;
#2468 = VERTEX_POINT ( 'NONE', #851 ) ;
#2469 = ORIENTED_EDGE ( 'NONE', *, *, #6408, .T. ) ;
#2470 = DIRECTION ( 'NONE',  ( -1.000000000000000000, 0.000000000000000000, -0.000000000000000000 ) ) ;
#2471 = CARTESIAN_POINT ( 'NONE',  ( -2.000000000000009770, 3.464101615137749057, -2.700000000000001066 ) ) ;
#2472 = DIRECTION ( 'NONE',  ( 0.000000000000000000, 0.000000000000000000, 1.000000000000000000 ) ) ;
#2473 = CARTESIAN_POINT ( 'NONE',  ( -3.499085248937321868, -6.067035836480215494, 8.008459478482038207 ) ) ;
#2474 = CARTESIAN_POINT ( 'NONE',  ( 1.810035846748221600, 6.765851833681423066, 8.002237581049140402 ) ) ;
#2475 = SHAPE_REPRESENTATION ( 'base', ( #1587 ), #517 ) ;
#2476 = ORIENTED_EDGE ( 'NONE', *, *, #8182, .F. ) ;
#2477 = ORIENTED_EDGE ( 'NONE', *, *, #820, .T. ) ;
#2478 = VECTOR ( 'NONE', #1651, 1000.000000000000000 ) ;
#2479 = CIRCLE ( 'NONE', #3151, 1.599999999999998979 ) ;
#2480 = CARTESIAN_POINT ( 'NONE',  ( -2.500000000000002220, 3.061616997868386099E-16, -25.03750572909317285 ) ) ;
#2481 = DIRECTION ( 'NONE',  ( -1.000000000000000000, 0.000000000000000000, -0.000000000000000000 ) ) ;
#2482 = DIRECTION ( 'NONE',  ( 0.000000000000000000, 0.000000000000000000, -1.000000000000000000 ) ) ;
#2483 = DIRECTION ( 'NONE',  ( -0.000000000000000000, -0.000000000000000000, 1.000000000000000000 ) ) ;
#2484 = LINE ( 'NONE', #6218, #242 ) ;
#2485 = CARTESIAN_POINT ( 'NONE',  ( 0.000000000000000000, 0.000000000000000000, 0.000000000000000000 ) ) ;
#2486 = ORIENTED_EDGE ( 'NONE', *, *, #4341, .T. ) ;
#2487 = DIRECTION ( 'NONE',  ( 0.000000000000000000, -0.4999999999999993339, 0.8660254037844389297 ) ) ;
#2488 = CARTESIAN_POINT ( 'NONE',  ( 2.000000000000000000, 0.8865213383406685965, -1.535500000000000753 ) ) ;
#2489 = DIRECTION ( 'NONE',  ( 0.000000000000000000, 0.000000000000000000, 1.000000000000000000 ) ) ;
#2490 = CARTESIAN_POINT ( 'NONE',  ( -3.345653888883663551, 2.687187980154699840, -2.560849780464863557 ) ) ;
#2491 = CARTESIAN_POINT ( 'NONE',  ( -4.000000000000000000, 0.7862748000878055921, -0.03447227762756575886 ) ) ;
#2492 = EDGE_CURVE ( 'NONE', #6378, #1969, #7214, .T. ) ;
#2493 = CARTESIAN_POINT ( 'NONE',  ( 49.97874610126637407, 86.47445480916304916, 1.919346332466817406 ) ) ;
#2494 = EDGE_CURVE ( 'NONE', #821, #7449, #5439, .T. ) ;
#2495 = ORIENTED_EDGE ( 'NONE', *, *, #7453, .T. ) ;
#2496 = ADVANCED_FACE ( 'NONE', ( #3455 ), #4191, .F. ) ;
#2497 = VECTOR ( 'NONE', #5226, 1000.000000000000114 ) ;
#2498 = ORIENTED_EDGE ( 'NONE', *, *, #7821, .T. ) ;
#2499 = DIRECTION ( 'NONE',  ( 1.000000000000000000, 0.000000000000000000, 0.000000000000000000 ) ) ;
#2500 = PRODUCT_DEFINITION_CONTEXT ( 'detailed design', #1960, 'design' ) ;
#2501 = EDGE_LOOP ( 'NONE', ( #5348, #4507, #3919, #4076 ) ) ;
#2502 = ORIENTED_EDGE ( 'NONE', *, *, #942, .F. ) ;
#2503 = CARTESIAN_POINT ( 'NONE',  ( 9.020562075079396891E-14, 10.00000000000000000, 729.2499999999977263 ) ) ;
#2504 = AXIS2_PLACEMENT_3D ( 'NONE', #2864, #2288, #2950 ) ;
#2505 = LINE ( 'NONE', #627, #5061 ) ;
#2506 = DIRECTION ( 'NONE',  ( 0.000000000000000000, 0.000000000000000000, 1.000000000000000000 ) ) ;
#2507 = B_SPLINE_CURVE_WITH_KNOTS ( 'NONE', 3,
 ( #1409, #5314, #5922, #1689, #2183, #3516 ),
 .UNSPECIFIED., .F., .F.,
 ( 4, 2, 4 ),
 ( 0.002336974151641575941, 0.003500975885716452358, 0.004664977619791328342 ),
 .UNSPECIFIED. ) ;
#2508 = FILL_AREA_STYLE ('',( #5502 ) ) ;
#2509 = VECTOR ( 'NONE', #5743, 1000.000000000000000 ) ;
#2510 = VERTEX_POINT ( 'NONE', #2197 ) ;
#2511 = DIRECTION ( 'NONE',  ( 0.000000000000000000, 0.000000000000000000, 1.000000000000000000 ) ) ;
#2512 = ORIENTED_EDGE ( 'NONE', *, *, #725, .T. ) ;
#2513 = VERTEX_POINT ( 'NONE', #947 ) ;
#2514 = CIRCLE ( 'NONE', #5043, 2.149999999999995470 ) ;
#2516 = LINE ( 'NONE', #3266, #7031 ) ;
#2515 = VECTOR ( 'NONE', #307, 1000.000000000000000 ) ;
#2517 = CARTESIAN_POINT ( 'NONE',  ( 41.96116023364841396, 86.80803686473167602, -1.583454828100570255 ) ) ;
#2518 = DIRECTION ( 'NONE',  ( -0.000000000000000000, -0.000000000000000000, 1.000000000000000000 ) ) ;
#2520 = EDGE_CURVE ( 'NONE', #2793, #5096, #234, .T. ) ;
#2519 = PRESENTATION_STYLE_ASSIGNMENT (( #6295 ) ) ;
#2521 = CARTESIAN_POINT ( 'NONE',  ( -1.813645741666879641, -6.764847328847696240, 8.002246981198915421 ) ) ;
#2522 = DIRECTION ( 'NONE',  ( -1.000000000000000000, -0.000000000000000000, -0.000000000000000000 ) ) ;
#2523 = AXIS2_PLACEMENT_3D ( 'NONE', #3499, #5906, #7771 ) ;
#2524 = AXIS2_PLACEMENT_3D ( 'NONE', #1862, #1054, #2965 ) ;
#2525 = EDGE_CURVE ( 'NONE', #166, #2355, #1086, .T. ) ;
#2526 = ORIENTED_EDGE ( 'NONE', *, *, #3007, .T. ) ;
#2527 = ORIENTED_EDGE ( 'NONE', *, *, #667, .T. ) ;
#2528 = CARTESIAN_POINT ( 'NONE',  ( 4.000000000000000000, 0.000000000000000000, 0.000000000000000000 ) ) ;
#2529 = FACE_BOUND ( 'NONE', #7810, .T. ) ;
#2530 = CARTESIAN_POINT ( 'NONE',  ( 3.000000000000002665, 0.000000000000000000, 0.000000000000000000 ) ) ;
#2531 = DIRECTION ( 'NONE',  ( -0.000000000000000000, -0.000000000000000000, 1.000000000000000000 ) ) ;
#2532 = CIRCLE ( 'NONE', #252, 4.999999999999997335 ) ;
#2533 = VECTOR ( 'NONE', #1281, 1000.000000000000000 ) ;
#2534 = DIRECTION ( 'NONE',  ( -0.000000000000000000, 1.000000000000000000, -0.000000000000000000 ) ) ;
#2535 = CARTESIAN_POINT ( 'NONE',  ( 0.000000000000000000, 1.773042676681340968, -2.276824562219559311E-15 ) ) ;
#2536 = PRODUCT_DEFINITION_SHAPE ( 'NONE', 'NONE',  #8208 ) ;
#2537 = COLOUR_RGB ( '', 0.66274510, 0.83137255, 0.94901961) ;
#2538 = CIRCLE ( 'NONE', #6083, 0.1000000000000000472 ) ;
#2539 = EDGE_LOOP ( 'NONE', ( #3915, #624, #5716, #7688 ) ) ;
#2540 = CARTESIAN_POINT ( 'NONE',  ( -2.000000000000009770, 3.464101615137749057, 0.000000000000000000 ) ) ;
#2541 = APPLICATION_CONTEXT ( 'automotive_design' ) ;
#2542 = ADVANCED_FACE ( 'NONE', ( #2285 ), #7966, .F. ) ;
#2543 = CARTESIAN_POINT ( 'NONE',  ( 0.000000000000000000, 0.000000000000000000, -2.700000000000000178 ) ) ;
#2544 = CARTESIAN_POINT ( 'NONE',  ( 5.200000000000020606, 0.000000000000000000, -6.938893903907228378E-15 ) ) ;
#2545 = VECTOR ( 'NONE', #4053, 1000.000000000000000 ) ;
#2546 = CARTESIAN_POINT ( 'NONE',  ( 0.1999999999999987899, 0.000000000000000000, 0.000000000000000000 ) ) ;
#2547 = EDGE_CURVE ( 'NONE', #1258, #6761, #5112, .T. ) ;
#2548 = CARTESIAN_POINT ( 'NONE',  ( 49.96738998307159818, 86.80892218194638588, -1.585032901986132226 ) ) ;
#2549 = EDGE_LOOP ( 'NONE', ( #2046, #1224, #5787, #2867 ) ) ;
#2550 = EDGE_LOOP ( 'NONE', ( #3124, #4296 ) ) ;
#2551 = PRODUCT_RELATED_PRODUCT_CATEGORY ( 'part', '', ( #3129 ) ) ;
#2552 = CARTESIAN_POINT ( 'NONE',  ( 41.99758845363990645, 84.53527270025752216, 2.357482664457419830 ) ) ;
#2553 = VERTEX_POINT ( 'NONE', #988 ) ;
#2554 = EDGE_LOOP ( 'NONE', ( #6971, #1629, #7451, #3710, #429, #1418 ) ) ;
#2555 = CARTESIAN_POINT ( 'NONE',  ( 2.000000000000000000, 1.773042676681340968, -2.276824562219559311E-15 ) ) ;
#2556 = CARTESIAN_POINT ( 'NONE',  ( 5.200000000000020606, 0.000000000000000000, -2.700000000000007727 ) ) ;
#2557 = CARTESIAN_POINT ( 'NONE',  ( 2.000000000000000000, 0.000000000000000000, 0.000000000000000000 ) ) ;
#2558 = VERTEX_POINT ( 'NONE', #3618 ) ;
#2559 = CARTESIAN_POINT ( 'NONE',  ( -2.678494666091065124, -3.072372537026388351, -2.665789719053451634 ) ) ;
#2560 = VERTEX_POINT ( 'NONE', #5405 ) ;
#2561 = EDGE_CURVE ( 'NONE', #471, #2701, #2861, .T. ) ;
#2562 = VERTEX_POINT ( 'NONE', #4819 ) ;
#2563 = EDGE_CURVE ( 'NONE', #5522, #3297, #1623, .T. ) ;
#2564 = CARTESIAN_POINT ( 'NONE',  ( 2.500000000000002220, -1.178949249685218970, -2.041999999999998483 ) ) ;
#2565 = LINE ( 'NONE', #6996, #5192 ) ;
#2566 = DIRECTION ( 'NONE',  ( 0.000000000000000000, 0.000000000000000000, -1.000000000000000000 ) ) ;
#2567 = AXIS2_PLACEMENT_3D ( 'NONE', #4143, #5319, #4687 ) ;
#2568 = FILL_AREA_STYLE_COLOUR ( '', #4158 ) ;
#2569 = CARTESIAN_POINT ( 'NONE',  ( 1.270137496355039850E-14, 85.00000000000011369, 5.000000000000046185 ) ) ;
#2570 = ADVANCED_FACE ( 'NONE', ( #4694 ), #4071, .F. ) ;
#2571 = ORIENTED_EDGE ( 'NONE', *, *, #5994, .F. ) ;
#2572 = CARTESIAN_POINT ( 'NONE',  ( -7.000000000000000000, 0.000000000000000000, 8.000000000000000000 ) ) ;
#2573 = DIRECTION ( 'NONE',  ( 1.000000000000000000, 0.000000000000000000, 0.000000000000000000 ) ) ;
#2574 = LINE ( 'NONE', #4635, #3706 ) ;
#2575 = FACE_OUTER_BOUND ( 'NONE', #3094, .T. ) ;
#2576 = CYLINDRICAL_SURFACE ( 'NONE', #2020, 4.250000000000000000 ) ;
#2577 = PRODUCT_DEFINITION_FORMATION_WITH_SPECIFIED_SOURCE ( 'ANY', '', #2317, .NOT_KNOWN. ) ;
#2578 = CARTESIAN_POINT ( 'NONE',  ( -49.94236053903777162, 87.40012995604533330, 0.1563225272305456826 ) ) ;
#2579 = ORIENTED_EDGE ( 'NONE', *, *, #5761, .F. ) ;
#2580 = CARTESIAN_POINT ( 'NONE',  ( 0.000000000000000000, 0.000000000000000000, 0.000000000000000000 ) ) ;
#2581 = SURFACE_STYLE_FILL_AREA ( #768 ) ;
#2582 = DIRECTION ( 'NONE',  ( -1.000000000000000000, -0.000000000000000000, -0.000000000000000000 ) ) ;
#2583 =( GEOMETRIC_REPRESENTATION_CONTEXT ( 3 ) GLOBAL_UNCERTAINTY_ASSIGNED_CONTEXT ( ( #8018 ) ) GLOBAL_UNIT_ASSIGNED_CONTEXT ( ( #468, #3002, #5014 ) ) REPRESENTATION_CONTEXT ( 'NONE', 'WORKASPACE' ) );
#2584 = CARTESIAN_POINT ( 'NONE',  ( 57.99999999999999289, 7.999999999999996447, 11.99999999999998934 ) ) ;
#2585 = DIRECTION ( 'NONE',  ( -0.000000000000000000, -0.000000000000000000, 1.000000000000000000 ) ) ;
#2586 = ORIENTED_EDGE ( 'NONE', *, *, #4702, .T. ) ;
#2587 = EDGE_CURVE ( 'NONE', #1297, #5522, #4947, .T. ) ;
#2588 = COLOUR_RGB ( '', 0.40784314, 0.44705882, 0.49803922) ;
#2589 = ORIENTED_EDGE ( 'NONE', *, *, #5700, .T. ) ;
#2590 = ADVANCED_FACE ( 'NONE', ( #7843 ), #7259, .F. ) ;
#2591 = CARTESIAN_POINT ( 'NONE',  ( 30.00000000000000000, 2.054999999999997939, -6.938893903907228378E-15 ) ) ;
#2592 = ADVANCED_FACE ( 'NONE', ( #7222 ), #5451, .F. ) ;
#2593 = VERTEX_POINT ( 'NONE', #4858 ) ;
#2594 = ORIENTED_EDGE ( 'NONE', *, *, #2171, .F. ) ;
#2595 = DIRECTION ( 'NONE',  ( 1.000000000000000000, 0.000000000000000000, 0.000000000000000000 ) ) ;
#2596 = AXIS2_PLACEMENT_3D ( 'NONE', #3358, #1486, #1560 ) ;
#2597 = DIRECTION ( 'NONE',  ( 0.000000000000000000, 0.000000000000000000, -1.000000000000000000 ) ) ;
#2598 = DIRECTION ( 'NONE',  ( -0.000000000000000000, -0.000000000000000000, -1.000000000000000000 ) ) ;
#2599 = B_SPLINE_CURVE_WITH_KNOTS ( 'NONE', 3,
 ( #1920, #7054, #5653, #2540 ),
 .UNSPECIFIED., .F., .F.,
 ( 4, 4 ),
 ( 2.380737581620913884E-07, 0.002336974151641539512 ),
 .UNSPECIFIED. ) ;
#2600 = CARTESIAN_POINT ( 'NONE',  ( 54.99999999999990052, 41.51196202519723499, 14.00000000000000000 ) ) ;
#2601 = ORIENTED_EDGE ( 'NONE', *, *, #303, .T. ) ;
#2602 = ORIENTED_EDGE ( 'NONE', *, *, #718, .F. ) ;
#2603 = EDGE_LOOP ( 'NONE', ( #5942, #1428, #4473, #6361 ) ) ;
#2604 = CARTESIAN_POINT ( 'NONE',  ( 2.500000000000002220, 3.061616997868386099E-16, -2.674599999999998978 ) ) ;
#2605 = DIRECTION ( 'NONE',  ( 0.000000000000000000, -0.4999999999999992784, 0.8660254037844390407 ) ) ;
#2606 = PLANE ( 'NONE',  #6198 ) ;
#2607 =( NAMED_UNIT ( * ) PLANE_ANGLE_UNIT ( ) SI_UNIT ( $, .RADIAN. ) );
#2608 = EDGE_CURVE ( 'NONE', #4530, #5459, #7385, .T. ) ;
#2609 = ORIENTED_EDGE ( 'NONE', *, *, #4925, .T. ) ;
#2610 = CARTESIAN_POINT ( 'NONE',  ( 50.00000000000003553, 85.00000000000012790, 5.000000000000045297 ) ) ;
#2611 = DIRECTION ( 'NONE',  ( 0.000000000000000000, 0.000000000000000000, -1.000000000000000000 ) ) ;
#2612 = EDGE_CURVE ( 'NONE', #3286, #6468, #2286, .T. ) ;
#2613 = CARTESIAN_POINT ( 'NONE',  ( 2.000000000000000000, 1.773042676681340968, -2.276824562219559311E-15 ) ) ;
#2614 = PLANE ( 'NONE',  #870 ) ;
#2615 = VECTOR ( 'NONE', #331, 1000.000000000000114 ) ;
#2616 = ORIENTED_EDGE ( 'NONE', *, *, #1539, .F. ) ;
#2617 = LINE ( 'NONE', #1880, #4043 ) ;
#2618 = LINE ( 'NONE', #7642, #617 ) ;
#2619 = FACE_OUTER_BOUND ( 'NONE', #5236, .T. ) ;
#2620 = DIRECTION ( 'NONE',  ( 0.000000000000000000, 0.000000000000000000, 1.000000000000000000 ) ) ;
#2621 = EDGE_CURVE ( 'NONE', #2626, #4815, #5978, .T. ) ;
#2622 = ORIENTED_EDGE ( 'NONE', *, *, #7234, .T. ) ;
#2623 = VERTEX_POINT ( 'NONE', #2411 ) ;
#2624 = CARTESIAN_POINT ( 'NONE',  ( 9.020562075079396891E-14, 10.00000000000000000, 8.000000000000007105 ) ) ;
#2625 = ORIENTED_EDGE ( 'NONE', *, *, #1211, .F. ) ;
#2626 = VERTEX_POINT ( 'NONE', #7513 ) ;
#2627 =( REPRESENTATION_RELATIONSHIP ('NONE','NONE', #3916, #3059 ) REPRESENTATION_RELATIONSHIP_WITH_TRANSFORMATION ( #1155 )SHAPE_REPRESENTATION_RELATIONSHIP( ) );
#2628 = CARTESIAN_POINT ( 'NONE',  ( 2.000000000000000000, 1.773042676681340968, -2.276824562219559311E-15 ) ) ;
#2629 = CARTESIAN_POINT ( 'NONE',  ( -54.99999999999990052, -10.00000000000000000, 15.49999999999877254 ) ) ;
#2630 = DIRECTION ( 'NONE',  ( -1.000000000000000000, -3.552713678800500929E-15, 0.000000000000000000 ) ) ;
#2631 = DIRECTION ( 'NONE',  ( 4.893789003257370080E-18, -2.081668171172168513E-17, -1.000000000000000000 ) ) ;
#2632 = ORIENTED_EDGE ( 'NONE', *, *, #2211, .T. ) ;
#2633 = MECHANICAL_DESIGN_GEOMETRIC_PRESENTATION_REPRESENTATION (  '', ( #1557 ), #3295 ) ;
#2634 = ORIENTED_EDGE ( 'NONE', *, *, #5972, .F. ) ;
#2635 = EDGE_LOOP ( 'NONE', ( #5794, #6445, #51, #3105 ) ) ;
#2636 = PLANE ( 'NONE',  #6488 ) ;
#2637 = CARTESIAN_POINT ( 'NONE',  ( 41.96471864142488073, 86.72849413951723818, 1.684781847096518792 ) ) ;
#2638 = DIRECTION ( 'NONE',  ( -0.000000000000000000, -0.000000000000000000, -1.000000000000000000 ) ) ;
#2639 = CONICAL_SURFACE ( 'NONE', #4494, 1.219500000000000028, 0.7853981633974680410 ) ;
#2640 = VECTOR ( 'NONE', #3843, 1000.000000000000114 ) ;
#2641 = CARTESIAN_POINT ( 'NONE',  ( -5.271109574984434332, -4.628614387250548745, 8.019189290563998540 ) ) ;
#2642 = AXIS2_PLACEMENT_3D ( 'NONE', #6817, #4792, #8055 ) ;
#2643 = AXIS2_PLACEMENT_3D ( 'NONE', #2825, #536, #4952 ) ;
#2644 = AXIS2_PLACEMENT_3D ( 'NONE', #568, #3110, #3648 ) ;
#2645 = PRODUCT_RELATED_PRODUCT_CATEGORY ( 'part', '', ( #5585 ) ) ;
#2646 = AXIS2_PLACEMENT_3D ( 'NONE', #4950, #2449, #3616 ) ;
#2647 = DIRECTION ( 'NONE',  ( 7.304098846218136639E-16, 0.000000000000000000, 1.000000000000000000 ) ) ;
#2648 = EDGE_CURVE ( 'NONE', #4584, #2013, #3077, .T. ) ;
#2649 = DIRECTION ( 'NONE',  ( -0.000000000000000000, -0.000000000000000000, -1.000000000000000000 ) ) ;
#2650 = CARTESIAN_POINT ( 'NONE',  ( 29.55500000000002458, 0.000000000000000000, -6.938893903907228378E-15 ) ) ;
#2651 = AXIS2_PLACEMENT_3D ( 'NONE', #3854, #4466, #3770 ) ;
#2652 = STYLED_ITEM ( 'NONE', ( #3425 ), #6832 ) ;
#2653 = CARTESIAN_POINT ( 'NONE',  ( 52.00000000000000711, 8.000000000000000000, 0.000000000000000000 ) ) ;
#2654 = CARTESIAN_POINT ( 'NONE',  ( -49.97864901397259985, 86.46689848149772217, 1.906053348878929077 ) ) ;
#2655 = VECTOR ( 'NONE', #6758, 1000.000000000000114 ) ;
#2656 = ORIENTED_EDGE ( 'NONE', *, *, #2929, .T. ) ;
#2657 = CARTESIAN_POINT ( 'NONE',  ( 55.00000000000000000, 10.00000000000000000, -6.149999999999981704 ) ) ;
#2658 = AXIS2_PLACEMENT_3D ( 'NONE', #7823, #1603, #7938 ) ;
#2659 = VECTOR ( 'NONE', #2483, 1000.000000000000000 ) ;
#2660 = DIRECTION ( 'NONE',  ( -1.000000000000000000, 0.000000000000000000, 0.000000000000000000 ) ) ;
#2661 = FACE_OUTER_BOUND ( 'NONE', #8158, .T. ) ;
#2662 = LINE ( 'NONE', #2696, #916 ) ;
#2663 = ORIENTED_EDGE ( 'NONE', *, *, #6259, .F. ) ;
#2664 = CIRCLE ( 'NONE', #2642, 721.2499999999977263 ) ;
#2665 = EDGE_CURVE ( 'NONE', #244, #8139, #5751, .T. ) ;
#2666 = AXIS2_PLACEMENT_3D ( 'NONE', #1804, #3289, #3221 ) ;
#2667 = ORIENTED_EDGE ( 'NONE', *, *, #3459, .T. ) ;
#2668 = LINE ( 'NONE', #3839, #7939 ) ;
#2669 = ORIENTED_EDGE ( 'NONE', *, *, #1889, .F. ) ;
#2670 = ORIENTED_EDGE ( 'NONE', *, *, #2525, .F. ) ;
#2671 = DIRECTION ( 'NONE',  ( 0.000000000000000000, 0.000000000000000000, -1.000000000000000000 ) ) ;
#2672 = CARTESIAN_POINT ( 'NONE',  ( 0.000000000000000000, 0.000000000000000000, -2.700000000000000178 ) ) ;
#2673 = APPLICATION_PROTOCOL_DEFINITION ( 'draft international standard', 'automotive_design', 1998, #6771 ) ;
#2674 = ORIENTED_EDGE ( 'NONE', *, *, #776, .F. ) ;
#2675 = ORIENTED_EDGE ( 'NONE', *, *, #253, .T. ) ;
#2676 = ORIENTED_EDGE ( 'NONE', *, *, #6190, .T. ) ;
#2677 = CARTESIAN_POINT ( 'NONE',  ( 1.300000000000000044, -1.108512516844082141, -0.6399999999999991251 ) ) ;
#2678 = CARTESIAN_POINT ( 'NONE',  ( 41.93504501510003735, 82.66492853475577363, 0.5690079308735644936 ) ) ;
#2679 = CARTESIAN_POINT ( 'NONE',  ( -39.83716857408418122, 108.0000000000001421, 4.163336342344337027E-14 ) ) ;
#2680 = SURFACE_STYLE_USAGE ( .BOTH. , #5259 ) ;
#2681 = ADVANCED_FACE ( 'NONE', ( #6935, #577 ), #2360, .T. ) ;
#2682 = ADVANCED_FACE ( 'NONE', ( #6312, #8170 ), #1152, .F. ) ;
#2683 = EDGE_CURVE ( 'NONE', #5862, #7730, #6790, .T. ) ;
#2684 = VECTOR ( 'NONE', #1027, 1000.000000000000000 ) ;
#2685 = CARTESIAN_POINT ( 'NONE',  ( 0.000000000000000000, 0.000000000000000000, 18.00000000000000355 ) ) ;
#2686 = CARTESIAN_POINT ( 'NONE',  ( 3.000000000000002665, 0.000000000000000000, 2.750000000000000000 ) ) ;
#2687 = DIRECTION ( 'NONE',  ( -0.000000000000000000, -0.000000000000000000, 1.000000000000000000 ) ) ;
#2688 = CARTESIAN_POINT ( 'NONE',  ( 55.00000000000000000, 10.00000000000000000, 15.50000000000000355 ) ) ;
#2689 = DIRECTION ( 'NONE',  ( 0.000000000000000000, 0.000000000000000000, 1.000000000000000000 ) ) ;
#2690 = AXIS2_PLACEMENT_3D ( 'NONE', #3430, #970, #4800 ) ;
#2691 = ORIENTED_EDGE ( 'NONE', *, *, #5402, .F. ) ;
#2692 = CARTESIAN_POINT ( 'NONE',  ( -60.00000000000000000, -10.00000000000000000, 20.00000000000000355 ) ) ;
#2693 = CARTESIAN_POINT ( 'NONE',  ( 5.000000000000015099, 0.000000000000000000, 0.000000000000000000 ) ) ;
#2694 = DIRECTION ( 'NONE',  ( 0.000000000000000000, 0.000000000000000000, -1.000000000000000000 ) ) ;
#2695 = DIRECTION ( 'NONE',  ( 1.000000000000000000, 0.000000000000000000, 0.000000000000000000 ) ) ;
#2696 = CARTESIAN_POINT ( 'NONE',  ( 60.00000000000000711, -10.00000000000000000, 0.000000000000000000 ) ) ;
#2697 = PRODUCT_DEFINITION_FORMATION_WITH_SPECIFIED_SOURCE ( 'ANY', '', #600, .NOT_KNOWN. ) ;
#2698 = EDGE_CURVE ( 'NONE', #4304, #2418, #5342, .T. ) ;
#2699 = ORIENTED_EDGE ( 'NONE', *, *, #485, .T. ) ;
#2700 = CARTESIAN_POINT ( 'NONE',  ( 49.95347202886240012, 82.84263588727935712, -1.063116165656391221 ) ) ;
#2701 = VERTEX_POINT ( 'NONE', #6272 ) ;
#2702 = VERTEX_POINT ( 'NONE', #4953 ) ;
#2703 = MECHANICAL_DESIGN_GEOMETRIC_PRESENTATION_REPRESENTATION (  '', ( #6950 ), #2583 ) ;
#2704 = CARTESIAN_POINT ( 'NONE',  ( 2.000000000000000000, 0.8865213383406685965, -1.535500000000000753 ) ) ;
#2705 = DIRECTION ( 'NONE',  ( 0.000000000000000000, 0.000000000000000000, -1.000000000000000000 ) ) ;
#2706 = EDGE_CURVE ( 'NONE', #4613, #7226, #3226, .T. ) ;
#2707 = CARTESIAN_POINT ( 'NONE',  ( 2.000000000000000000, 0.8865213383406685965, -1.535500000000000753 ) ) ;
#2708 = PRODUCT_CONTEXT ( 'NONE', #3818, 'mechanical' ) ;
#2709 = EDGE_CURVE ( 'NONE', #5103, #4940, #1765, .T. ) ;
#2710 = ORIENTED_EDGE ( 'NONE', *, *, #1809, .T. ) ;
#2711 = ORIENTED_EDGE ( 'NONE', *, *, #5389, .T. ) ;
#2712 = ORIENTED_EDGE ( 'NONE', *, *, #2492, .T. ) ;
#2713 = CARTESIAN_POINT ( 'NONE',  ( 24.00000000000000000, 0.000000000000000000, 1.610000000000000098 ) ) ;
#2714 = CARTESIAN_POINT ( 'NONE',  ( 5.566201872177863663, -4.269108285804360747, 8.021434216347806512 ) ) ;
#2715 = DIRECTION ( 'NONE',  ( 1.000000000000000000, 0.000000000000000000, 0.000000000000000000 ) ) ;
#2716 = CARTESIAN_POINT ( 'NONE',  ( -31.74999999999995737, 2.449293598294707893E-16, -2.000000000000000888 ) ) ;
#2717 = CARTESIAN_POINT ( 'NONE',  ( -31.74999999999994316, 0.000000000000000000, 0.000000000000000000 ) ) ;
#2718 =( NAMED_UNIT ( * ) PLANE_ANGLE_UNIT ( ) SI_UNIT ( $, .RADIAN. ) );
#2719 = CARTESIAN_POINT ( 'NONE',  ( 2.099999999999999645, 0.000000000000000000, -2.700000000000000178 ) ) ;
#2720 = DIRECTION ( 'NONE',  ( 1.000000000000000000, 0.000000000000000000, 0.000000000000000000 ) ) ;
#2721 = ORIENTED_EDGE ( 'NONE', *, *, #4889, .F. ) ;
#2722 = CARTESIAN_POINT ( 'NONE',  ( 1.300000000000000044, 1.108512516844080364, -0.6400000000000017897 ) ) ;
#2723 = DIRECTION ( 'NONE',  ( 0.000000000000000000, 0.5000000000000011102, 0.8660254037844379305 ) ) ;
#2724 = CARTESIAN_POINT ( 'NONE',  ( 2.650000000000006573, 0.000000000000000000, 14.60000000000000142 ) ) ;
#2725 = CYLINDRICAL_SURFACE ( 'NONE', #6206, 42.00000000000002132 ) ;
#2726 = CYLINDRICAL_SURFACE ( 'NONE', #5844, 2.099999999999999645 ) ;
#2727 = EDGE_CURVE ( 'NONE', #2846, #3286, #4335, .T. ) ;
#2728 = CYLINDRICAL_SURFACE ( 'NONE', #948, 3.500000000000000000 ) ;
#2729 = ORIENTED_EDGE ( 'NONE', *, *, #797, .T. ) ;
#2730 = CARTESIAN_POINT ( 'NONE',  ( 49.99422363137632885, 84.22622254513471773, -2.277283319317807031 ) ) ;
#2731 = PRESENTATION_LAYER_ASSIGNMENT (  '', '', ( #8099 ) ) ;
#2732 = UNCERTAINTY_MEASURE_WITH_UNIT (LENGTH_MEASURE( 1.000000000000000082E-05 ), #7276, 'distance_accuracy_value', 'NONE');
#2733 = EDGE_LOOP ( 'NONE', ( #2858, #5555, #7315 ) ) ;
#2734 = VERTEX_POINT ( 'NONE', #614 ) ;
#2735 = DIRECTION ( 'NONE',  ( 1.000000000000000000, 0.000000000000000000, 0.000000000000000000 ) ) ;
#2736 = EDGE_CURVE ( 'NONE', #1038, #4949, #5219, .T. ) ;
#2737 = CIRCLE ( 'NONE', #3150, 2.649999999999999467 ) ;
#2738 = VECTOR ( 'NONE', #1697, 1000.000000000000000 ) ;
#2739 = DIRECTION ( 'NONE',  ( 0.000000000000000000, 0.000000000000000000, 1.000000000000000000 ) ) ;
#2740 = EDGE_CURVE ( 'NONE', #3297, #5311, #2808, .T. ) ;
#2741 = EDGE_CURVE ( 'NONE', #2418, #2397, #1363, .T. ) ;
#2742 = DIRECTION ( 'NONE',  ( -1.000000000000000000, 0.000000000000000000, 0.000000000000000000 ) ) ;
#2743 = ITEM_DEFINED_TRANSFORMATION ( 'NONE', 'NONE', #3914,  #1587 ) ;
#2744 = EDGE_CURVE ( 'NONE', #8139, #2810, #5988, .T. ) ;
#2745 = ORIENTED_EDGE ( 'NONE', *, *, #6483, .F. ) ;
#2746 = ORIENTED_EDGE ( 'NONE', *, *, #7323, .F. ) ;
#2747 = ORIENTED_EDGE ( 'NONE', *, *, #529, .T. ) ;
#2748 = DIRECTION ( 'NONE',  ( 0.000000000000000000, 0.000000000000000000, 1.000000000000000000 ) ) ;
#2749 = CARTESIAN_POINT ( 'NONE',  ( 2.253877478482040786, -6.643060962426256211, 8.003397232069101364 ) ) ;
#2750 = CARTESIAN_POINT ( 'NONE',  ( 60.00000000000000711, 10.00000000000000000, 60.00000000000000000 ) ) ;
#2751 = AXIS2_PLACEMENT_3D ( 'NONE', #7856, #4705, #1546 ) ;
#2752 = COLOUR_RGB ( '', 0.31764706, 0.68627451, 0.89019608) ;
#2753 = CARTESIAN_POINT ( 'NONE',  ( 39.83716857408421674, 108.0000000000001990, -4.999999999999976907 ) ) ;
#2754 = CIRCLE ( 'NONE', #7774, 0.2000000000000000944 ) ;
#2755 = VECTOR ( 'NONE', #3438, 1000.000000000000000 ) ;
#2756 = EDGE_CURVE ( 'NONE', #2818, #2258, #3472, .T. ) ;
#2757 = CARTESIAN_POINT ( 'NONE',  ( 5.000000000000015099, 0.000000000000000000, 0.000000000000000000 ) ) ;
#2758 = CYLINDRICAL_SURFACE ( 'NONE', #2255, 1.249999999999998446 ) ;
#2759 =( NAMED_UNIT ( * ) SI_UNIT ( $, .STERADIAN. ) SOLID_ANGLE_UNIT ( ) );
#2760 = FACE_OUTER_BOUND ( 'NONE', #7981, .T. ) ;
#2761 = CLOSED_SHELL ( 'NONE', ( #4611, #3360, #6732, #971, #6074, #5441, #2830, #738, #105, #2406, #504, #7061, #2910, #7538, #8011, #3103, #1163, #5698, #2570, #2230, #2972, #2932, #1034, #5744, #4629, #1236, #2785 ) ) ;
#2762 = AXIS2_PLACEMENT_3D ( 'NONE', #2693, #3279, #5854 ) ;
#2763 = DIRECTION ( 'NONE',  ( 0.000000000000000000, 0.000000000000000000, 1.000000000000000000 ) ) ;
#2764 = CONICAL_SURFACE ( 'NONE', #5948, 2.055000000000000160, 0.7853981633974717047 ) ;
#2765 = ORIENTED_EDGE ( 'NONE', *, *, #4048, .F. ) ;
#2766 = CARTESIAN_POINT ( 'NONE',  ( 0.000000000000000000, 1.478016689125442484, -1.626303258728256651E-15 ) ) ;
#2767 = DIRECTION ( 'NONE',  ( -1.000000000000000000, 0.000000000000000000, 0.000000000000000000 ) ) ;
#2768 = CARTESIAN_POINT ( 'NONE',  ( 55.00000000000000000, 10.00000000000000000, 13.35000000000000853 ) ) ;
#2769 = AXIS2_PLACEMENT_3D ( 'NONE', #4992, #7512, #2359 ) ;
#2770 = CIRCLE ( 'NONE', #4368, 2.099999999999999645 ) ;
#2771 = CARTESIAN_POINT ( 'NONE',  ( 0.000000000000000000, 0.000000000000000000, 0.000000000000000000 ) ) ;
#2772 = CARTESIAN_POINT ( 'NONE',  ( 11.00000000000000355, 0.000000000000000000, 1.219500000000000028 ) ) ;
#2773 = VECTOR ( 'NONE', #6170, 1000.000000000000000 ) ;
#2774 = DIRECTION ( 'NONE',  ( 0.000000000000000000, 0.000000000000000000, 1.000000000000000000 ) ) ;
#2775 = EDGE_LOOP ( 'NONE', ( #7152, #1759, #4915, #2999, #1669 ) ) ;
#2776 = CIRCLE ( 'NONE', #7418, 2.500000000000000444 ) ;
#2777 = DIRECTION ( 'NONE',  ( -1.000000000000000000, -0.000000000000000000, -0.000000000000000000 ) ) ;
#2778 = AXIS2_PLACEMENT_3D ( 'NONE', #367, #413, #2955 ) ;
#2779 = VERTEX_POINT ( 'NONE', #447 ) ;
#2780 = ADVANCED_FACE ( 'NONE', ( #5529 ), #8043, .T. ) ;
#2781 = AXIS2_PLACEMENT_3D ( 'NONE', #4338, #4389, #8068 ) ;
#2782 = EDGE_LOOP ( 'NONE', ( #7659, #7484, #6677, #6945 ) ) ;
#2783 = AXIS2_PLACEMENT_3D ( 'NONE', #7248, #2187, #7336 ) ;
#2784 = DIRECTION ( 'NONE',  ( 0.000000000000000000, -1.000000000000000000, 0.000000000000000000 ) ) ;
#2785 = ADVANCED_FACE ( 'NONE', ( #3658 ), #4196, .F. ) ;
#2786 = DIRECTION ( 'NONE',  ( 0.000000000000000000, 0.5000000000000013323, 0.8660254037844378194 ) ) ;
#2787 = LINE ( 'NONE', #5330, #5420 ) ;
#2788 = CARTESIAN_POINT ( 'NONE',  ( -58.00000000000006395, 7.999999999999996447, 11.99999999999998934 ) ) ;
#2789 = VECTOR ( 'NONE', #496, 1000.000000000000000 ) ;
#2790 = PRODUCT_DEFINITION ( 'UNKNOWN', '', #5640, #7573 ) ;
#2791 = ORIENTED_EDGE ( 'NONE', *, *, #5357, .T. ) ;
#2792 = STYLED_ITEM ( 'NONE', ( #2800 ), #1401 ) ;
#2793 = VERTEX_POINT ( 'NONE', #4566 ) ;
#2794 = VERTEX_POINT ( 'NONE', #7173 ) ;
#2795 = DIRECTION ( 'NONE',  ( 1.412205397084881070E-17, -2.775557561562891967E-17, -1.000000000000000000 ) ) ;
#2796 = APPLICATION_CONTEXT ( 'automotive_design' ) ;
#2797 = CARTESIAN_POINT ( 'NONE',  ( 6.643161419842083859, -2.253695319827236254, 8.030573092606642760 ) ) ;
#2798 = DIRECTION ( 'NONE',  ( 1.412205397084881070E-17, -2.775557561562891967E-17, -1.000000000000000000 ) ) ;
#2799 = AXIS2_PLACEMENT_3D ( 'NONE', #6035, #878, #3984 ) ;
#2800 = PRESENTATION_STYLE_ASSIGNMENT (( #141 ) ) ;
#2801 = EDGE_CURVE ( 'NONE', #8121, #3249, #5040, .T. ) ;
#2802 = EDGE_CURVE ( 'NONE', #3217, #4315, #3245, .T. ) ;
#2803 = CARTESIAN_POINT ( 'NONE',  ( -31.74999999999995737, 0.000000000000000000, 2.750000000000000000 ) ) ;
#2804 = CARTESIAN_POINT ( 'NONE',  ( 11.00000000000000355, 0.000000000000000000, 0.000000000000000000 ) ) ;
#2805 = EDGE_CURVE ( 'NONE', #4315, #117, #733, .T. ) ;
#2806 = LINE ( 'NONE', #2719, #5730 ) ;
#2807 = DIRECTION ( 'NONE',  ( 0.000000000000000000, 0.000000000000000000, 1.000000000000000000 ) ) ;
#2808 = CIRCLE ( 'NONE', #277, 2.000000000000000888 ) ;
#2809 = EDGE_LOOP ( 'NONE', ( #5930, #3009, #681, #7461 ) ) ;
#2810 = VERTEX_POINT ( 'NONE', #663 ) ;
#2811 = DIRECTION ( 'NONE',  ( -0.000000000000000000, -0.000000000000000000, 1.000000000000000000 ) ) ;
#2812 = CARTESIAN_POINT ( 'NONE',  ( -52.00000000000006395, -8.000000000000003553, 11.99999999999998934 ) ) ;
#2813 = CARTESIAN_POINT ( 'NONE',  ( -41.94160807294379367, 87.21436019787591931, 0.9342823132686582932 ) ) ;
#2814 = DIRECTION ( 'NONE',  ( 0.000000000000000000, 1.000000000000000000, -0.000000000000000000 ) ) ;
#2815 = FACE_OUTER_BOUND ( 'NONE', #1868, .T. ) ;
#2816 = AXIS2_PLACEMENT_3D ( 'NONE', #3749, #537, #8135 ) ;
#2817 = CARTESIAN_POINT ( 'NONE',  ( 0.000000000000000000, 0.000000000000000000, -2.394516984716111185 ) ) ;
#2818 = VERTEX_POINT ( 'NONE', #6461 ) ;
#2819 = DIRECTION ( 'NONE',  ( -0.000000000000000000, -0.000000000000000000, -1.000000000000000000 ) ) ;
#2820 = VERTEX_POINT ( 'NONE', #3831 ) ;
#2821 = ORIENTED_EDGE ( 'NONE', *, *, #150, .T. ) ;
#2822 = DIRECTION ( 'NONE',  ( 1.000000000000000000, 2.168404344971008621E-16, -0.000000000000000000 ) ) ;
#2823 = DIRECTION ( 'NONE',  ( 0.000000000000000000, -0.5000000000000009992, -0.8660254037844380415 ) ) ;
#2824 = CARTESIAN_POINT ( 'NONE',  ( 30.00000000000001066, -29.99999999999997868, 10.00000000000000000 ) ) ;
#2825 = CARTESIAN_POINT ( 'NONE',  ( 0.000000000000000000, 0.000000000000000000, 10.00000000000000000 ) ) ;
#2826 = CARTESIAN_POINT ( 'NONE',  ( 2.500000000000002220, -2.357898499370430834, 3.469446951953614189E-15 ) ) ;
#2827 = DIRECTION ( 'NONE',  ( -0.000000000000000000, -0.000000000000000000, 1.000000000000000000 ) ) ;
#2828 = APPLICATION_PROTOCOL_DEFINITION ( 'draft international standard', 'automotive_design', 1998, #5776 ) ;
#2829 = ADVANCED_FACE ( 'NONE', ( #110, #3328 ), #6355, .T. ) ;
#2830 = ADVANCED_FACE ( 'NONE', ( #2072, #3280 ), #7095, .T. ) ;
#2831 = VERTEX_POINT ( 'NONE', #5778 ) ;
#2832 = EDGE_LOOP ( 'NONE', ( #2203, #6719, #3807, #7702, #7394 ) ) ;
#2833 = ORIENTED_EDGE ( 'NONE', *, *, #7159, .F. ) ;
#2834 = LINE ( 'NONE', #5256, #6753 ) ;
#2835 = FACE_OUTER_BOUND ( 'NONE', #5212, .T. ) ;
#2836 = DIRECTION ( 'NONE',  ( -1.000000000000000000, -0.000000000000000000, -0.000000000000000000 ) ) ;
#2837 =( NAMED_UNIT ( * ) PLANE_ANGLE_UNIT ( ) SI_UNIT ( $, .RADIAN. ) );
#2838 = CARTESIAN_POINT ( 'NONE',  ( 2.000000000000000000, -1.773042676681340524, 1.734723475976807094E-15 ) ) ;
#2839 = EDGE_CURVE ( 'NONE', #5534, #5475, #812, .T. ) ;
#2840 = EDGE_CURVE ( 'NONE', #7486, #3462, #2754, .T. ) ;
#2841 = DIRECTION ( 'NONE',  ( -1.000000000000000000, 0.000000000000000000, 1.412205397084726379E-17 ) ) ;
#2842 =( NAMED_UNIT ( * ) PLANE_ANGLE_UNIT ( ) SI_UNIT ( $, .RADIAN. ) );
#2843 = AXIS2_PLACEMENT_3D ( 'NONE', #932, #6575, #3476 ) ;
#2844 = FACE_OUTER_BOUND ( 'NONE', #3641, .T. ) ;
#2845 = CARTESIAN_POINT ( 'NONE',  ( 1.084202172485504434E-14, 4.618802153517020948, -2.342734410091827701 ) ) ;
#2846 = VERTEX_POINT ( 'NONE', #1451 ) ;
#2847 = VERTEX_POINT ( 'NONE', #3992 ) ;
#2848 = DIRECTION ( 'NONE',  ( -1.000000000000000000, -0.000000000000000000, -0.000000000000000000 ) ) ;
#2849 = DIRECTION ( 'NONE',  ( -0.000000000000000000, -0.000000000000000000, 1.000000000000000000 ) ) ;
#2850 = LINE ( 'NONE', #934, #1006 ) ;
#2851 = DIRECTION ( 'NONE',  ( -1.000000000000000000, 0.000000000000000000, 0.000000000000000000 ) ) ;
#2852 = CARTESIAN_POINT ( 'NONE',  ( -1.198153218366585720E-14, 42.68016229225776925, 0.000000000000000000 ) ) ;
#2853 = CARTESIAN_POINT ( 'NONE',  ( -49.95669240716469517, 82.91758674606776935, -1.203334160065746339 ) ) ;
#2854 = DIRECTION ( 'NONE',  ( -1.000000000000000000, -1.502586498047605218E-16, 1.412205397084881070E-17 ) ) ;
#2855 = ORIENTED_EDGE ( 'NONE', *, *, #3372, .F. ) ;
#2856 = DIRECTION ( 'NONE',  ( -1.000000000000000000, -0.000000000000000000, -0.000000000000000000 ) ) ;
#2857 = ORIENTED_EDGE ( 'NONE', *, *, #6301, .F. ) ;
#2858 = ORIENTED_EDGE ( 'NONE', *, *, #482, .F. ) ;
#2859 = CARTESIAN_POINT ( 'NONE',  ( 0.000000000000000000, -0.8865213383406690406, 1.535500000000000975 ) ) ;
#2860 = CARTESIAN_POINT ( 'NONE',  ( 0.000000000000000000, 0.000000000000000000, 18.00000000000000355 ) ) ;
#2861 = LINE ( 'NONE', #5329, #417 ) ;
#2862 = EDGE_CURVE ( 'NONE', #3630, #972, #6048, .T. ) ;
#2863 = CARTESIAN_POINT ( 'NONE',  ( -6.639644148827243519, 2.263345988190933689, 8.030540921233406237 ) ) ;
#2864 = CARTESIAN_POINT ( 'NONE',  ( 0.000000000000000000, 0.000000000000000000, -0.2800830152838832965 ) ) ;
#2865 = APPLICATION_PROTOCOL_DEFINITION ( 'draft international standard', 'automotive_design', 1998, #7191 ) ;
#2866 = ORIENTED_EDGE ( 'NONE', *, *, #6995, .F. ) ;
#2867 = ORIENTED_EDGE ( 'NONE', *, *, #82, .T. ) ;
#2868 = AXIS2_PLACEMENT_3D ( 'NONE', #3767, #5717, #3332 ) ;
#2869 = ORIENTED_EDGE ( 'NONE', *, *, #5232, .T. ) ;
#2870 = DIRECTION ( 'NONE',  ( 0.000000000000000000, 0.000000000000000000, 1.000000000000000000 ) ) ;
#2871 = CARTESIAN_POINT ( 'NONE',  ( 9.020562075079396891E-14, -10.00000000000000000, 8.000000000000007105 ) ) ;
#2872 = DIRECTION ( 'NONE',  ( 0.000000000000000000, 1.000000000000000000, -1.467581828789149532E-15 ) ) ;
#2873 =( NAMED_UNIT ( * ) PLANE_ANGLE_UNIT ( ) SI_UNIT ( $, .RADIAN. ) );
#2874 = ORIENTED_EDGE ( 'NONE', *, *, #2683, .F. ) ;
#2875 = CARTESIAN_POINT ( 'NONE',  ( 1.300000000000000044, -0.7390083445627225744, -1.279999999999999138 ) ) ;
#2876 = EDGE_CURVE ( 'NONE', #7000, #4888, #2737, .T. ) ;
#2877 = ADVANCED_FACE ( 'NONE', ( #5206, #769, #5742 ), #3361, .F. ) ;
#2878 = DIRECTION ( 'NONE',  ( 0.000000000000000000, 0.000000000000000000, -1.000000000000000000 ) ) ;
#2879 = LINE ( 'NONE', #6565, #7033 ) ;
#2880 = DIRECTION ( 'NONE',  ( -0.000000000000000000, -0.000000000000000000, 1.000000000000000000 ) ) ;
#2881 = UNCERTAINTY_MEASURE_WITH_UNIT (LENGTH_MEASURE( 1.000000000000000082E-05 ), #1183, 'distance_accuracy_value', 'NONE');
#2882 = CARTESIAN_POINT ( 'NONE',  ( 1.318516776095787879, 3.857556137907072635, -2.700000000000003730 ) ) ;
#2883 = CIRCLE ( 'NONE', #8047, 2.149999999999995470 ) ;
#2884 = PRODUCT_DEFINITION ( 'UNKNOWN', '', #7087, #582 ) ;
#2885 = AXIS2_PLACEMENT_3D ( 'NONE', #6211, #1237, #6833 ) ;
#2886 = ORIENTED_EDGE ( 'NONE', *, *, #8204, .T. ) ;
#2887 = ORIENTED_EDGE ( 'NONE', *, *, #6394, .F. ) ;
#2888 = DIRECTION ( 'NONE',  ( 0.000000000000000000, 0.000000000000000000, -1.000000000000000000 ) ) ;
#2889 = COLOUR_RGB ( '', 0.72549020, 0.75294118, 0.79215686) ;
#2890 = DIRECTION ( 'NONE',  ( 0.000000000000000000, -0.000000000000000000, 1.000000000000000000 ) ) ;
#2891 = LINE ( 'NONE', #1015, #4865 ) ;
#2892 = DIRECTION ( 'NONE',  ( -1.000000000000000000, 0.000000000000000000, 0.000000000000000000 ) ) ;
#2893 = CARTESIAN_POINT ( 'NONE',  ( 29.99999999999997868, 30.00000000000001421, 4.599999999999997868 ) ) ;
#2894 = CARTESIAN_POINT ( 'NONE',  ( -49.94600989915083744, 82.67684773840545631, -0.6225708050467673171 ) ) ;
#2895 = VECTOR ( 'NONE', #219, 1000.000000000000000 ) ;
#2896 = VECTOR ( 'NONE', #1705, 1000.000000000000000 ) ;
#2897 = CARTESIAN_POINT ( 'NONE',  ( -60.00000000000000000, -10.00000000000000000, 20.00000000000000355 ) ) ;
#2898 = EDGE_LOOP ( 'NONE', ( #1902, #1266, #2372 ) ) ;
#2899 = CARTESIAN_POINT ( 'NONE',  ( 60.00000000000014211, -10.00000000000000000, 10.50000000000006395 ) ) ;
#2900 = VERTEX_POINT ( 'NONE', #2724 ) ;
#2901 = AXIS2_PLACEMENT_3D ( 'NONE', #3178, #5052, #2464 ) ;
#2902 = EDGE_LOOP ( 'NONE', ( #3475, #808 ) ) ;
#2903 = CIRCLE ( 'NONE', #1044, 1.610000000000000098 ) ;
#2904 = CARTESIAN_POINT ( 'NONE',  ( 5.860087342385653250E-15, 38.99999999999999289, 0.000000000000000000 ) ) ;
#2905 = CIRCLE ( 'NONE', #5045, 42.00000000000002132 ) ;
#2906 = FACE_OUTER_BOUND ( 'NONE', #1415, .T. ) ;
#2907 = CARTESIAN_POINT ( 'NONE',  ( 4.000000000000000000, 0.000000000000000000, -2.700000000000001066 ) ) ;
#2908 = CARTESIAN_POINT ( 'NONE',  ( 60.00000000000000711, -10.00000000000000000, 60.00000000000000000 ) ) ;
#2909 = DIRECTION ( 'NONE',  ( 0.000000000000000000, 0.000000000000000000, 1.000000000000000000 ) ) ;
#2910 = ADVANCED_FACE ( 'NONE', ( #68 ), #8035, .F. ) ;
#2911 = AXIS2_PLACEMENT_3D ( 'NONE', #5224, #2748, #246 ) ;
#2912 = ORIENTED_EDGE ( 'NONE', *, *, #2520, .T. ) ;
#2913 = VECTOR ( 'NONE', #4311, 1000.000000000000000 ) ;
#2914 = ORIENTED_EDGE ( 'NONE', *, *, #3294, .T. ) ;
#2915 = ORIENTED_EDGE ( 'NONE', *, *, #3565, .F. ) ;
#2916 = DIRECTION ( 'NONE',  ( -1.000000000000000000, -0.000000000000000000, -0.000000000000000000 ) ) ;
#2917 = CARTESIAN_POINT ( 'NONE',  ( 2.000000000000000000, -0.8865213383406721492, -1.535499999999999199 ) ) ;
#2918 = VECTOR ( 'NONE', #4201, 1000.000000000000000 ) ;
#2919 = PLANE ( 'NONE',  #1974 ) ;
#2920 = ORIENTED_EDGE ( 'NONE', *, *, #6168, .F. ) ;
#2921 = DIRECTION ( 'NONE',  ( 0.000000000000000000, 0.000000000000000000, 1.000000000000000000 ) ) ;
#2922 = VECTOR ( 'NONE', #514, 1000.000000000000000 ) ;
#2923 = ORIENTED_EDGE ( 'NONE', *, *, #3134, .T. ) ;
#2924 = VECTOR ( 'NONE', #1951, 1000.000000000000114 ) ;
#2925 = AXIS2_PLACEMENT_3D ( 'NONE', #1517, #1483, #5345 ) ;
#2926 = DIRECTION ( 'NONE',  ( 0.000000000000000000, 0.000000000000000000, 1.000000000000000000 ) ) ;
#2927 = CARTESIAN_POINT ( 'NONE',  ( 2.500000000000002220, 1.178949249685212086, -2.042000000000002036 ) ) ;
#2928 = CARTESIAN_POINT ( 'NONE',  ( 2.000000000000000000, 0.8865213383406687075, -1.535500000000000975 ) ) ;
#2929 = EDGE_CURVE ( 'NONE', #4177, #1617, #3949, .T. ) ;
#2930 = EDGE_CURVE ( 'NONE', #479, #5129, #2618, .T. ) ;
#2931 = DIRECTION ( 'NONE',  ( -1.000000000000000000, -0.000000000000000000, -0.000000000000000000 ) ) ;
#2932 = ADVANCED_FACE ( 'NONE', ( #4846 ), #344, .F. ) ;
#2933 = ORIENTED_EDGE ( 'NONE', *, *, #4581, .F. ) ;
#2934 = ORIENTED_EDGE ( 'NONE', *, *, #3030, .T. ) ;
#2935 = CARTESIAN_POINT ( 'NONE',  ( 60.00000000000000711, -10.00000000000000000, 19.99999999999998224 ) ) ;
#2936 = PLANE ( 'NONE',  #205 ) ;
#2937 = CARTESIAN_POINT ( 'NONE',  ( -41.93161561614412847, 87.39575111243146921, 0.1913511295312773086 ) ) ;
#2938 = DIRECTION ( 'NONE',  ( 0.000000000000000000, 0.000000000000000000, 1.000000000000000000 ) ) ;
#2939 = DIRECTION ( 'NONE',  ( 0.000000000000000000, 1.000000000000000000, -1.026972870230479989E-15 ) ) ;
#2940 = CARTESIAN_POINT ( 'NONE',  ( 1.300000000000000044, -0.7390083445627200209, 1.280000000000001137 ) ) ;
#2941 = ORIENTED_EDGE ( 'NONE', *, *, #4363, .F. ) ;
#2942 = DIRECTION ( 'NONE',  ( -0.000000000000000000, -0.000000000000000000, 1.000000000000000000 ) ) ;
#2943 = EDGE_LOOP ( 'NONE', ( #2337, #7091 ) ) ;
#2944 = VERTEX_POINT ( 'NONE', #7954 ) ;
#2945 = CARTESIAN_POINT ( 'NONE',  ( -3.999999999999999112, 1.557668341133520373, -2.540303434304243879 ) ) ;
#2946 = DIRECTION ( 'NONE',  ( 1.000000000000000000, 2.775557561562890365E-16, -1.734723475976806478E-17 ) ) ;
#2947 = DIRECTION ( 'NONE',  ( 0.000000000000000000, 0.000000000000000000, 1.000000000000000000 ) ) ;
#2948 = AXIS2_PLACEMENT_3D ( 'NONE', #6681, #6104, #6767 ) ;
#2949 = CARTESIAN_POINT ( 'NONE',  ( 0.000000000000000000, -2.357898499370430834, 3.469446951953614189E-15 ) ) ;
#2950 = DIRECTION ( 'NONE',  ( 1.000000000000000000, 0.000000000000000000, 0.000000000000000000 ) ) ;
#2951 = CONTEXT_DEPENDENT_SHAPE_REPRESENTATION ( #5718, #6905 ) ;
#2952 = EDGE_LOOP ( 'NONE', ( #6085, #7583, #7151, #4345 ) ) ;
#2953 = ORIENTED_EDGE ( 'NONE', *, *, #7801, .F. ) ;
#2954 = ORIENTED_EDGE ( 'NONE', *, *, #8069, .T. ) ;
#2955 = DIRECTION ( 'NONE',  ( 0.000000000000000000, 0.000000000000000000, 1.000000000000000000 ) ) ;
#2956 = CARTESIAN_POINT ( 'NONE',  ( 55.00000000000000000, 10.00000000000000000, 13.35000000000000853 ) ) ;
#2957 = DIRECTION ( 'NONE',  ( -1.000000000000000000, 0.000000000000000000, 2.065146995210483462E-17 ) ) ;
#2958 = ADVANCED_FACE ( 'NONE', ( #2271 ), #4681, .T. ) ;
#2959 = UNCERTAINTY_MEASURE_WITH_UNIT (LENGTH_MEASURE( 1.000000000000000082E-05 ), #5067, 'distance_accuracy_value', 'NONE');
#2960 = VERTEX_POINT ( 'NONE', #2812 ) ;
#2961 = LINE ( 'NONE', #4206, #5001 ) ;
#2962 = ORIENTED_EDGE ( 'NONE', *, *, #2989, .T. ) ;
#2963 = ORIENTED_EDGE ( 'NONE', *, *, #5726, .T. ) ;
#2964 = CARTESIAN_POINT ( 'NONE',  ( 42.00000000000003553, 85.00000000000049738, 2.399999999999971934 ) ) ;
#2965 = DIRECTION ( 'NONE',  ( 0.000000000000000000, 0.000000000000000000, -1.000000000000000000 ) ) ;
#2966 = EDGE_CURVE ( 'NONE', #4874, #1855, #2850, .T. ) ;
#2967 = AXIS2_PLACEMENT_3D ( 'NONE', #7528, #1848, #4379 ) ;
#2968 = LINE ( 'NONE', #5514, #281 ) ;
#2969 = VERTEX_POINT ( 'NONE', #264 ) ;
#2970 = ORIENTED_EDGE ( 'NONE', *, *, #201, .T. ) ;
#2971 = AXIS2_PLACEMENT_3D ( 'NONE', #4804, #4136, #1610 ) ;
#2972 = ADVANCED_FACE ( 'NONE', ( #6709 ), #2936, .F. ) ;
#2973 = CARTESIAN_POINT ( 'NONE',  ( -41.93508307841045024, 87.33455813751852759, -0.5710001583726183050 ) ) ;
#2974 = DIRECTION ( 'NONE',  ( -0.000000000000000000, -0.000000000000000000, 1.000000000000000000 ) ) ;
#2975 = LINE ( 'NONE', #5519, #1873 ) ;
#2976 = FACE_OUTER_BOUND ( 'NONE', #579, .T. ) ;
#2977 = DIRECTION ( 'NONE',  ( -0.000000000000000000, 0.000000000000000000, -1.000000000000000000 ) ) ;
#2978 = PRODUCT_DEFINITION_SHAPE ( 'NONE', 'NONE',  #8211 ) ;
#2979 = ORIENTED_EDGE ( 'NONE', *, *, #6953, .T. ) ;
#2980 = ORIENTED_EDGE ( 'NONE', *, *, #4924, .F. ) ;
#2981 = DIRECTION ( 'NONE',  ( -1.000000000000000000, 0.000000000000000000, 1.412205397084881070E-17 ) ) ;
#2982 = FACE_OUTER_BOUND ( 'NONE', #32, .T. ) ;
#2983 = DIRECTION ( 'NONE',  ( 1.000000000000000000, 0.000000000000000000, 0.000000000000000000 ) ) ;
#2984 = DIRECTION ( 'NONE',  ( 0.000000000000000000, 0.000000000000000000, 1.000000000000000000 ) ) ;
#2985 = ORIENTED_EDGE ( 'NONE', *, *, #2741, .F. ) ;
#2986 = EDGE_CURVE ( 'NONE', #117, #1235, #1525, .T. ) ;
#2987 = ORIENTED_EDGE ( 'NONE', *, *, #7974, .T. ) ;
#2988 = EDGE_LOOP ( 'NONE', ( #7756, #8019, #6112, #1210, #7036, #7651, #1121, #3848 ) ) ;
#2989 = EDGE_CURVE ( 'NONE', #8142, #2468, #6668, .T. ) ;
#2990 = DIRECTION ( 'NONE',  ( -1.000000000000000000, -0.000000000000000000, -0.000000000000000000 ) ) ;
#2991 = CARTESIAN_POINT ( 'NONE',  ( 2.886521338340684917, 0.000000000000000000, 0.000000000000000000 ) ) ;
#2992 = DIRECTION ( 'NONE',  ( 0.000000000000000000, 1.000000000000000000, -0.000000000000000000 ) ) ;
#2993 = EDGE_CURVE ( 'NONE', #4127, #7254, #2891, .T. ) ;
#2994 = SURFACE_STYLE_USAGE ( .BOTH. , #2465 ) ;
#2995 = ORIENTED_EDGE ( 'NONE', *, *, #1770, .T. ) ;
#2996 = CARTESIAN_POINT ( 'NONE',  ( 32.64999999999997726, 30.00000000000001421, 4.599999999999997868 ) ) ;
#2997 = VECTOR ( 'NONE', #2819, 1000.000000000000000 ) ;
#2998 = ORIENTED_EDGE ( 'NONE', *, *, #6498, .T. ) ;
#2999 = ORIENTED_EDGE ( 'NONE', *, *, #6775, .F. ) ;
#3000 = CARTESIAN_POINT ( 'NONE',  ( -54.99999999999990052, 10.00000000000000000, 15.49999999999877254 ) ) ;
#3001 = CARTESIAN_POINT ( 'NONE',  ( -41.97224725382100274, 83.45833230446734774, 1.857373340501012660 ) ) ;
#3002 =( NAMED_UNIT ( * ) PLANE_ANGLE_UNIT ( ) SI_UNIT ( $, .RADIAN. ) );
#3003 = PLANE ( 'NONE',  #6111 ) ;
#3004 = ADVANCED_FACE ( 'NONE', ( #3391 ), #1292, .T. ) ;
#3005 = CARTESIAN_POINT ( 'NONE',  ( 3.104279414096060119, 6.290759372240700031, 8.006556128919173787 ) ) ;
#3006 = EDGE_CURVE ( 'NONE', #189, #2779, #5433, .T. ) ;
#3007 = EDGE_CURVE ( 'NONE', #6705, #4315, #7990, .T. ) ;
#3008 = VERTEX_POINT ( 'NONE', #2184 ) ;
#3009 = ORIENTED_EDGE ( 'NONE', *, *, #6153, .T. ) ;
#3010 =( NAMED_UNIT ( * ) PLANE_ANGLE_UNIT ( ) SI_UNIT ( $, .RADIAN. ) );
#3011 = DIRECTION ( 'NONE',  ( 1.000000000000000000, 0.000000000000000000, 0.000000000000000000 ) ) ;
#3012 = DIRECTION ( 'NONE',  ( 0.000000000000000000, -1.000000000000000000, 0.000000000000000000 ) ) ;
#3013 = CARTESIAN_POINT ( 'NONE',  ( -4.000000000000000000, 0.000000000000000000, -2.700000000000000178 ) ) ;
#3014 = CIRCLE ( 'NONE', #755, 721.2499999999977263 ) ;
#3015 = CARTESIAN_POINT ( 'NONE',  ( -3.469446951953613006E-15, 0.000000000000000000, 1.040834085586084257E-14 ) ) ;
#3016 = AXIS2_PLACEMENT_3D ( 'NONE', #4805, #3477, #7370 ) ;
#3017 = CARTESIAN_POINT ( 'NONE',  ( 35.00000000000000000, -29.99999999999997868, 4.599999999999997868 ) ) ;
#3018 = ORIENTED_EDGE ( 'NONE', *, *, #1137, .T. ) ;
#3019 = AXIS2_PLACEMENT_3D ( 'NONE', #7184, #5174, #7070 ) ;
#3020 = ORIENTED_EDGE ( 'NONE', *, *, #4793, .T. ) ;
#3021 = CARTESIAN_POINT ( 'NONE',  ( 2.000000000000000000, 1.773042676681340968, -2.276824562219559311E-15 ) ) ;
#3022 = DIRECTION ( 'NONE',  ( 0.000000000000000000, 0.000000000000000000, -1.000000000000000000 ) ) ;
#3023 = LINE ( 'NONE', #6227, #3976 ) ;
#3024 = DIRECTION ( 'NONE',  ( -1.000000000000000000, 0.000000000000000000, 1.032573497605241731E-17 ) ) ;
#3025 = AXIS2_PLACEMENT_3D ( 'NONE', #3739, #3781, #474 ) ;
#3026 = LINE ( 'NONE', #7386, #2896 ) ;
#3027 = LINE ( 'NONE', #8098, #6203 ) ;
#3028 = ORIENTED_EDGE ( 'NONE', *, *, #801, .T. ) ;
#3029 = AXIS2_PLACEMENT_3D ( 'NONE', #4377, #5137, #7619 ) ;
#3030 = EDGE_CURVE ( 'NONE', #8200, #5903, #6989, .T. ) ;
#3031 = CIRCLE ( 'NONE', #2769, 2.149999999999995470 ) ;
#3032 = AXIS2_PLACEMENT_3D ( 'NONE', #5899, #125, #6553 ) ;
#3033 = ORIENTED_EDGE ( 'NONE', *, *, #2621, .T. ) ;
#3034 = ADVANCED_FACE ( 'NONE', ( #5923 ), #4600, .T. ) ;
#3035 = AXIS2_PLACEMENT_3D ( 'NONE', #1789, #4903, #6889 ) ;
#3036 = ORIENTED_EDGE ( 'NONE', *, *, #2993, .F. ) ;
#3037 = EDGE_LOOP ( 'NONE', ( #7751, #2601, #7521, #5999 ) ) ;
#3038 = DIRECTION ( 'NONE',  ( 0.000000000000000000, 1.000000000000000000, -1.103561164596346103E-15 ) ) ;
#3039 = CARTESIAN_POINT ( 'NONE',  ( -39.99999999999999289, 40.00000000000000711, 10.00000000000000000 ) ) ;
#3040 = DIRECTION ( 'NONE',  ( 0.000000000000000000, 0.000000000000000000, 1.000000000000000000 ) ) ;
#3041 = AXIS2_PLACEMENT_3D ( 'NONE', #1003, #1731, #8113 ) ;
#3042 = VECTOR ( 'NONE', #1614, 1000.000000000000000 ) ;
#3043 = ORIENTED_EDGE ( 'NONE', *, *, #2665, .F. ) ;
#3044 = DIRECTION ( 'NONE',  ( 1.000000000000000000, 0.000000000000000000, 0.000000000000000000 ) ) ;
#3045 = CONICAL_SURFACE ( 'NONE', #6494, 2.060000000000000941, 0.9599310885968777018 ) ;
#3046 = ORIENTED_EDGE ( 'NONE', *, *, #505, .T. ) ;
#3047 = VERTEX_POINT ( 'NONE', #4762 ) ;
#3048 = AXIS2_PLACEMENT_3D ( 'NONE', #8014, #4249, #2374 ) ;
#3049 = AXIS2_PLACEMENT_3D ( 'NONE', #5012, #1092, #6744 ) ;
#3050 = CIRCLE ( 'NONE', #7569, 1.250000000000001110 ) ;
#3051 = DIRECTION ( 'NONE',  ( 0.000000000000000000, 1.000000000000000000, -1.100686371591861952E-15 ) ) ;
#3052 = CARTESIAN_POINT ( 'NONE',  ( -41.98244464128907794, 83.78046611586739800, -2.071021427375471902 ) ) ;
#3053 = EDGE_CURVE ( 'NONE', #7269, #4852, #8173, .T. ) ;
#3054 = PRODUCT_DEFINITION_SHAPE ( 'NONE', 'NONE',  #8207 ) ;
#3055 = CARTESIAN_POINT ( 'NONE',  ( 0.1499999999999973577, 0.000000000000000000, 0.000000000000000000 ) ) ;
#3057 = EDGE_CURVE ( 'NONE', #6951, #4508, #6625, .T. ) ;
#3056 = VECTOR ( 'NONE', #7356, 1000.000000000000000 ) ;
#3058 = PLANE ( 'NONE',  #3764 ) ;
#3059 = SHAPE_REPRESENTATION ( 'socket head cap screw_iso_ISO 4762 M3 x 8 - 8N', ( #1587 ), #3111 ) ;
#3060 = VERTEX_POINT ( 'NONE', #6577 ) ;
#3061 = STYLED_ITEM ( 'NONE', ( #1907 ), #1362 ) ;
#3062 = ORIENTED_EDGE ( 'NONE', *, *, #4415, .T. ) ;
#3063 = EDGE_CURVE ( 'NONE', #7949, #5123, #2146, .T. ) ;
#3064 = CARTESIAN_POINT ( 'NONE',  ( 50.00000000000000000, -10.00000000000000000, 60.00000000000000000 ) ) ;
#3065 = CARTESIAN_POINT ( 'NONE',  ( -3.469446951953613006E-15, 0.000000000000000000, 20.00000000000000355 ) ) ;
#3066 = DIRECTION ( 'NONE',  ( -1.000000000000000000, -0.000000000000000000, -0.000000000000000000 ) ) ;
#3067 =( REPRESENTATION_RELATIONSHIP ('NONE','NONE', #3916, #6413 ) REPRESENTATION_RELATIONSHIP_WITH_TRANSFORMATION ( #2743 )SHAPE_REPRESENTATION_RELATIONSHIP( ) );
#3068 = PLANE ( 'NONE',  #2256 ) ;
#3069 = AXIS2_PLACEMENT_3D ( 'NONE', #7088, #5081, #61 ) ;
#3070 = DIRECTION ( 'NONE',  ( 0.000000000000000000, 0.000000000000000000, 1.000000000000000000 ) ) ;
#3071 = CARTESIAN_POINT ( 'NONE',  ( -1.599999999999998757, 42.68016229225776925, 4.000000000000001776 ) ) ;
#3072 = ORIENTED_EDGE ( 'NONE', *, *, #2096, .F. ) ;
#3073 = EDGE_LOOP ( 'NONE', ( #4827, #714, #6402, #6165, #1497 ) ) ;
#3074 = CARTESIAN_POINT ( 'NONE',  ( -3.999999999999999112, 1.935983797701082976, -2.450530693383766501 ) ) ;
#3075 = CARTESIAN_POINT ( 'NONE',  ( -39.99999999999999289, 40.00000000000000711, 10.00000000000000000 ) ) ;
#3076 = DIRECTION ( 'NONE',  ( 0.000000000000000000, 0.000000000000000000, -1.000000000000000000 ) ) ;
#3077 = LINE ( 'NONE', #1792, #31 ) ;
#3078 = CARTESIAN_POINT ( 'NONE',  ( 0.000000000000000000, 37.49999999999999289, 0.000000000000000000 ) ) ;
#3079 = CARTESIAN_POINT ( 'NONE',  ( 49.97491191256678178, 86.58758952878010007, -1.806678789609242664 ) ) ;
#3080 = B_SPLINE_CURVE_WITH_KNOTS ( 'NONE', 3,
 ( #146, #3869, #5234, #5120, #7089, #6395, #3904, #4598, #6428, #3986, #5082, #1406, #3240, #1997, #4483, #2578, #4528, #6503, #7602, #693, #7052, #807, #6350, #3944, #2654, #6968, #1371, #1284, #656, #3205 ),
 .UNSPECIFIED., .F., .F.,
 ( 4, 2, 2, 2, 2, 2, 2, 2, 2, 2, 2, 2, 2, 2, 4 ),
 ( 0.007504573511820675745, 0.007973502549960232236, 0.008442431588099789594, 0.009380289664378940739, 0.009849218702518501567, 0.01031814774065806413, 0.01078707677879762669, 0.01125600581693718752, 0.01172493485507674835, 0.01219386389321631091, 0.01266279293135587347, 0.01313172196949543430, 0.01360065100763499513, 0.01406958004577455595, 0.01500743812205367934 ),
 .UNSPECIFIED. ) ;
#3081 = ORIENTED_EDGE ( 'NONE', *, *, #5141, .T. ) ;
#3082 = ORIENTED_EDGE ( 'NONE', *, *, #1684, .F. ) ;
#3083 = ORIENTED_EDGE ( 'NONE', *, *, #8017, .T. ) ;
#3084 = VECTOR ( 'NONE', #1616, 1000.000000000000000 ) ;
#3085 = VERTEX_POINT ( 'NONE', #7867 ) ;
#3086 = DIRECTION ( 'NONE',  ( 1.412205397084881070E-17, -2.775557561562891967E-17, -1.000000000000000000 ) ) ;
#3087 = CARTESIAN_POINT ( 'NONE',  ( 0.1499999999999973577, 0.000000000000000000, 0.000000000000000000 ) ) ;
#3088 = CYLINDRICAL_SURFACE ( 'NONE', #1449, 2.650000000000003020 ) ;
#3089 = DIRECTION ( 'NONE',  ( 1.000000000000000000, 0.000000000000000000, 0.000000000000000000 ) ) ;
#3090 = AXIS2_PLACEMENT_3D ( 'NONE', #5265, #1554, #6535 ) ;
#3091 = ORIENTED_EDGE ( 'NONE', *, *, #1938, .T. ) ;
#3092 = CARTESIAN_POINT ( 'NONE',  ( 10.00000000000000000, 1.224646799147353256E-15, 18.00000000000000355 ) ) ;
#3093 = VERTEX_POINT ( 'NONE', #1612 ) ;
#3094 = EDGE_LOOP ( 'NONE', ( #5982, #4998, #8076, #4419, #1505 ) ) ;
#3095 = FACE_OUTER_BOUND ( 'NONE', #2385, .T. ) ;
#3096 = CARTESIAN_POINT ( 'NONE',  ( 50.00000000000003553, 85.00000000000012790, 2.399999999999971489 ) ) ;
#3097 = CARTESIAN_POINT ( 'NONE',  ( 2.000000000000000000, 0.8865213383406685965, -1.535500000000000753 ) ) ;
#3098 = FILL_AREA_STYLE_COLOUR ( '', #5883 ) ;
#3099 = DIRECTION ( 'NONE',  ( 0.000000000000000000, 0.000000000000000000, 1.000000000000000000 ) ) ;
#3100 = CARTESIAN_POINT ( 'NONE',  ( 1.300000000000000044, 1.478016689125442484, -1.626303258728256651E-15 ) ) ;
#3101 =( GEOMETRIC_REPRESENTATION_CONTEXT ( 3 ) GLOBAL_UNCERTAINTY_ASSIGNED_CONTEXT ( ( #2959 ) ) GLOBAL_UNIT_ASSIGNED_CONTEXT ( ( #5067, #4299, #4469 ) ) REPRESENTATION_CONTEXT ( 'NONE', 'WORKASPACE' ) );
#3102 = EDGE_CURVE ( 'NONE', #5593, #6791, #6866, .T. ) ;
#3103 = ADVANCED_FACE ( 'NONE', ( #7591 ), #2606, .F. ) ;
#3104 = EDGE_LOOP ( 'NONE', ( #2373, #4277 ) ) ;
#3105 = ORIENTED_EDGE ( 'NONE', *, *, #5324, .T. ) ;
#3106 = EDGE_CURVE ( 'NONE', #1609, #6979, #5013, .T. ) ;
#3107 = CARTESIAN_POINT ( 'NONE',  ( -58.00000000000006395, 7.999999999999996447, 19.99999999999998934 ) ) ;
#3108 = DIRECTION ( 'NONE',  ( 0.000000000000000000, 0.000000000000000000, 1.000000000000000000 ) ) ;
#3109 = DIRECTION ( 'NONE',  ( -0.000000000000000000, -0.000000000000000000, 1.000000000000000000 ) ) ;
#3110 = DIRECTION ( 'NONE',  ( -1.000000000000000000, -0.000000000000000000, -0.000000000000000000 ) ) ;
#3111 =( GEOMETRIC_REPRESENTATION_CONTEXT ( 3 ) GLOBAL_UNCERTAINTY_ASSIGNED_CONTEXT ( ( #5895 ) ) GLOBAL_UNIT_ASSIGNED_CONTEXT ( ( #5909, #3418, #4741 ) ) REPRESENTATION_CONTEXT ( 'NONE', 'WORKASPACE' ) );
#3112 = DIRECTION ( 'NONE',  ( 0.000000000000000000, 0.000000000000000000, -1.000000000000000000 ) ) ;
#3113 = CARTESIAN_POINT ( 'NONE',  ( 0.000000000000000000, 0.8865213383406687075, -1.535500000000000975 ) ) ;
#3114 = ORIENTED_EDGE ( 'NONE', *, *, #7795, .F. ) ;
#3115 = AXIS2_PLACEMENT_3D ( 'NONE', #1605, #4934, #1478 ) ;
#3116 = LINE ( 'NONE', #2657, #7090 ) ;
#3117 = CARTESIAN_POINT ( 'NONE',  ( 2.000000000000010658, -3.464101615137748169, -2.700000000000001066 ) ) ;
#3118 = DIRECTION ( 'NONE',  ( 0.000000000000000000, 0.000000000000000000, 1.000000000000000000 ) ) ;
#3119 = CARTESIAN_POINT ( 'NONE',  ( -4.000000000000000000, -2.309401076758531346, -0.3572655899081733644 ) ) ;
#3120 = DIRECTION ( 'NONE',  ( 0.000000000000000000, 0.000000000000000000, 1.000000000000000000 ) ) ;
#3121 = CARTESIAN_POINT ( 'NONE',  ( 49.99637443241782364, 85.62167278847336149, 2.323444847100735178 ) ) ;
#3122 = AXIS2_PLACEMENT_3D ( 'NONE', #1522, #7752, #5388 ) ;
#3123 = EDGE_LOOP ( 'NONE', ( #4691, #3400, #3722, #1346, #6978 ) ) ;
#3124 = ORIENTED_EDGE ( 'NONE', *, *, #6407, .T. ) ;
#3125 = CARTESIAN_POINT ( 'NONE',  ( 2.650000000000003020, 3.245314017740489906E-16, 0.000000000000000000 ) ) ;
#3126 = ORIENTED_EDGE ( 'NONE', *, *, #5156, .T. ) ;
#3127 = EDGE_CURVE ( 'NONE', #3432, #5625, #7536, .T. ) ;
#3128 = EDGE_LOOP ( 'NONE', ( #5287, #2011, #2009, #3602 ) ) ;
#3129 = PRODUCT ( 'mirror holder', 'mirror holder', '', ( #2246 ) ) ;
#3130 = FACE_OUTER_BOUND ( 'NONE', #1887, .T. ) ;
#3131 = FACE_OUTER_BOUND ( 'NONE', #1619, .T. ) ;
#3132 = CARTESIAN_POINT ( 'NONE',  ( -39.99999999999999289, -39.99999999999999289, 0.000000000000000000 ) ) ;
#3133 =( NAMED_UNIT ( * ) SI_UNIT ( $, .STERADIAN. ) SOLID_ANGLE_UNIT ( ) );
#3134 = EDGE_CURVE ( 'NONE', #1966, #2318, #6293, .T. ) ;
#3135 = ORIENTED_EDGE ( 'NONE', *, *, #6415, .T. ) ;
#3136 = CARTESIAN_POINT ( 'NONE',  ( 49.95346277782375921, 82.84241399044236687, 1.062802698623439568 ) ) ;
#3137 = ORIENTED_EDGE ( 'NONE', *, *, #291, .F. ) ;
#3138 = ORIENTED_EDGE ( 'NONE', *, *, #325, .T. ) ;
#3139 = FACE_OUTER_BOUND ( 'NONE', #911, .T. ) ;
#3140 = CARTESIAN_POINT ( 'NONE',  ( -41.97907998747121638, 83.67059623091998333, -2.002229301367134617 ) ) ;
#3141 = DIRECTION ( 'NONE',  ( 1.000000000000000000, 0.000000000000000000, 0.000000000000000000 ) ) ;
#3142 = SURFACE_SIDE_STYLE ('',( #4340 ) ) ;
#3143 =( GEOMETRIC_REPRESENTATION_CONTEXT ( 3 ) GLOBAL_UNCERTAINTY_ASSIGNED_CONTEXT ( ( #4214 ) ) GLOBAL_UNIT_ASSIGNED_CONTEXT ( ( #3467, #5875, #802 ) ) REPRESENTATION_CONTEXT ( 'NONE', 'WORKASPACE' ) );
#3144 = CYLINDRICAL_SURFACE ( 'NONE', #6769, 7.000000000000000000 ) ;
#3145 = PLANE ( 'NONE',  #3353 ) ;
#3146 = EDGE_CURVE ( 'NONE', #7631, #2513, #2883, .T. ) ;
#3147 = EDGE_CURVE ( 'NONE', #5852, #4453, #6462, .T. ) ;
#3148 = EDGE_LOOP ( 'NONE', ( #6232, #4727, #272, #1100 ) ) ;
#3149 = VERTEX_POINT ( 'NONE', #1815 ) ;
#3150 = AXIS2_PLACEMENT_3D ( 'NONE', #3210, #3909, #699 ) ;
#3151 = AXIS2_PLACEMENT_3D ( 'NONE', #5650, #3651, #1243 ) ;
#3152 = LINE ( 'NONE', #1777, #640 ) ;
#3153 = PLANE ( 'NONE',  #5940 ) ;
#3154 = CARTESIAN_POINT ( 'NONE',  ( 2.000000000000000000, -1.329782007511006281, -0.7677499999999984892 ) ) ;
#3155 = DIRECTION ( 'NONE',  ( -1.000000000000000000, 0.000000000000000000, 0.000000000000000000 ) ) ;
#3156 = FACE_BOUND ( 'NONE', #2417, .T. ) ;
#3157 = LINE ( 'NONE', #4352, #2738 ) ;
#3158 = ORIENTED_EDGE ( 'NONE', *, *, #6836, .F. ) ;
#3159 = CARTESIAN_POINT ( 'NONE',  ( 2.000000000000010658, -3.464101615137748169, -2.700000000000001066 ) ) ;
#3160 = DIRECTION ( 'NONE',  ( 0.000000000000000000, 0.000000000000000000, 1.000000000000000000 ) ) ;
#3161 = CARTESIAN_POINT ( 'NONE',  ( -2.681483223904233881, 3.070647092368429032, -2.700000000000003730 ) ) ;
#3162 = CARTESIAN_POINT ( 'NONE',  ( 41.08716857408421674, 108.0000000000001990, -4.999999999999976907 ) ) ;
#3163 =( REPRESENTATION_RELATIONSHIP ('NONE','NONE', #3916, #2201 ) REPRESENTATION_RELATIONSHIP_WITH_TRANSFORMATION ( #7438 )SHAPE_REPRESENTATION_RELATIONSHIP( ) );
#3164 = CARTESIAN_POINT ( 'NONE',  ( 49.94237310791758944, 87.39986840612067454, 0.1602877778558433053 ) ) ;
#3165 = VERTEX_POINT ( 'NONE', #3232 ) ;
#3166 = EDGE_CURVE ( 'NONE', #7486, #7189, #5932, .T. ) ;
#3167 = AXIS2_PLACEMENT_3D ( 'NONE', #2679, #2798, #3302 ) ;
#3168 = VERTEX_POINT ( 'NONE', #3814 ) ;
#3169 = LINE ( 'NONE', #2624, #4241 ) ;
#3170 = PRODUCT_DEFINITION_CONTEXT ( 'detailed design', #927, 'design' ) ;
#3171 = CIRCLE ( 'NONE', #632, 1.250000000000001110 ) ;
#3172 = EDGE_LOOP ( 'NONE', ( #43, #6414, #5821, #8051 ) ) ;
#3173 = ORIENTED_EDGE ( 'NONE', *, *, #7410, .T. ) ;
#3174 = CARTESIAN_POINT ( 'NONE',  ( 24.99999999999998224, 30.00000000000001421, 4.599999999999997868 ) ) ;
#3175 = VECTOR ( 'NONE', #3493, 1000.000000000000000 ) ;
#3177 = ADVANCED_FACE ( 'NONE', ( #6997 ), #6335, .F. ) ;
#3176 = CARTESIAN_POINT ( 'NONE',  ( 0.000000000000000000, -1.178949249685215417, 2.042000000000002036 ) ) ;
#3178 = CARTESIAN_POINT ( 'NONE',  ( 55.00000000000000000, 10.00000000000000000, 15.50000000000000355 ) ) ;
#3179 = DIRECTION ( 'NONE',  ( 6.123233995736743849E-17, -1.000000000000000000, -1.363075293218144361E-18 ) ) ;
#3180 = CIRCLE ( 'NONE', #5294, 2.649999999999995914 ) ;
#3181 = VECTOR ( 'NONE', #8044, 1000.000000000000000 ) ;
#3182 = VERTEX_POINT ( 'NONE', #1311 ) ;
#3183 = DIRECTION ( 'NONE',  ( 0.000000000000000000, 0.000000000000000000, -1.000000000000000000 ) ) ;
#3184 = EDGE_LOOP ( 'NONE', ( #207, #1082, #4228, #198, #3410 ) ) ;
#3185 = ORIENTED_EDGE ( 'NONE', *, *, #5385, .F. ) ;
#3186 = VECTOR ( 'NONE', #3506, 1000.000000000000000 ) ;
#3188 = DIRECTION ( 'NONE',  ( 1.000000000000000000, 0.000000000000000000, 0.000000000000000000 ) ) ;
#3187 = AXIS2_PLACEMENT_3D ( 'NONE', #5734, #3109, #1104 ) ;
#3189 = CARTESIAN_POINT ( 'NONE',  ( 41.94160807294385762, 82.78563980212508966, 0.9342823132686682852 ) ) ;
#3190 = CARTESIAN_POINT ( 'NONE',  ( 1.300000000000000044, 0.7390083445627193548, -1.280000000000000693 ) ) ;
#3191 =( NAMED_UNIT ( * ) PLANE_ANGLE_UNIT ( ) SI_UNIT ( $, .RADIAN. ) );
#3192 = AXIS2_PLACEMENT_3D ( 'NONE', #581, #7024, #6278 ) ;
#3193 = CARTESIAN_POINT ( 'NONE',  ( 2.000000000000000000, 0.000000000000000000, 0.000000000000000000 ) ) ;
#3194 = CIRCLE ( 'NONE', #5191, 39.00000000000002132 ) ;
#3195 = CONICAL_SURFACE ( 'NONE', #1334, 1.535500000000000087, 1.047197551196590748 ) ;
#3196 = ORIENTED_EDGE ( 'NONE', *, *, #4960, .T. ) ;
#3197 = DIRECTION ( 'NONE',  ( 0.000000000000000000, -1.224646799147353207E-16, 1.000000000000000000 ) ) ;
#3198 = LINE ( 'NONE', #6925, #500 ) ;
#3199 = DIRECTION ( 'NONE',  ( -1.000000000000000000, -0.000000000000000000, -0.000000000000000000 ) ) ;
#3200 = ADVANCED_FACE ( 'NONE', ( #5109 ), #8191, .F. ) ;
#3201 = LINE ( 'NONE', #5117, #5301 ) ;
#3202 = VECTOR ( 'NONE', #6985, 1000.000000000000000 ) ;
#3203 = CARTESIAN_POINT ( 'NONE',  ( 2.500000000000002220, 1.178949249685212086, -2.042000000000002036 ) ) ;
#3204 = EDGE_CURVE ( 'NONE', #4768, #3881, #7533, .T. ) ;
#3205 = CARTESIAN_POINT ( 'NONE',  ( -49.99999999999999289, 85.00000000000005684, 2.400000000000013234 ) ) ;
#3206 = AXIS2_PLACEMENT_3D ( 'NONE', #469, #6746, #6125 ) ;
#3207 = ORIENTED_EDGE ( 'NONE', *, *, #8008, .T. ) ;
#3208 = DIRECTION ( 'NONE',  ( 0.000000000000000000, -0.5000000000000011102, -0.8660254037844379305 ) ) ;
#3209 = CYLINDRICAL_SURFACE ( 'NONE', #6080, 2.649999999999995914 ) ;
#3210 = CARTESIAN_POINT ( 'NONE',  ( -29.99999999999999289, 30.00000000000000711, 4.599999999999997868 ) ) ;
#3211 = AXIS2_PLACEMENT_3D ( 'NONE', #3470, #7200, #926 ) ;
#3212 = CARTESIAN_POINT ( 'NONE',  ( -4.000000000000000000, 0.000000000000000000, 0.000000000000000000 ) ) ;
#3213 = CARTESIAN_POINT ( 'NONE',  ( 49.94597403161979798, 87.32391958025814915, -0.6195456578939724235 ) ) ;
#3214 = ORIENTED_EDGE ( 'NONE', *, *, #3612, .F. ) ;
#3215 = ORIENTED_EDGE ( 'NONE', *, *, #6190, .F. ) ;
#3216 = DIRECTION ( 'NONE',  ( 1.412205397084881070E-17, -2.775557561562891967E-17, -1.000000000000000000 ) ) ;
#3217 = VERTEX_POINT ( 'NONE', #7662 ) ;
#3218 = EDGE_LOOP ( 'NONE', ( #5927, #5692 ) ) ;
#3219 = EDGE_CURVE ( 'NONE', #4714, #4852, #5679, .T. ) ;
#3220 = PLANE ( 'NONE',  #5295 ) ;
#3221 = DIRECTION ( 'NONE',  ( 1.000000000000000000, 0.000000000000000000, 0.000000000000000000 ) ) ;
#3222 = LINE ( 'NONE', #6858, #4366 ) ;
#3223 = DIRECTION ( 'NONE',  ( 1.000000000000000000, 1.363075293218191931E-18, 6.123233995736766036E-17 ) ) ;
#3224 = B_SPLINE_CURVE_WITH_KNOTS ( 'NONE', 3,
 ( #3574, #3454, #6014, #5365, #275, #1752 ),
 .UNSPECIFIED., .F., .F.,
 ( 4, 2, 4 ),
 ( 0.006456566858647416578, 0.007625406818786683791, 0.008794246778925951871 ),
 .UNSPECIFIED. ) ;
#3225 = ORIENTED_EDGE ( 'NONE', *, *, #2319, .F. ) ;
#3226 = B_SPLINE_CURVE_WITH_KNOTS ( 'NONE', 3,
 ( #8096, #2490, #3161, #4319 ),
 .UNSPECIFIED., .F., .F.,
 ( 4, 4 ),
 ( 2.380737581781596034E-07, 0.002336974151641540379 ),
 .UNSPECIFIED. ) ;
#3227 = VERTEX_POINT ( 'NONE', #686 ) ;
#3228 = ORIENTED_EDGE ( 'NONE', *, *, #1770, .F. ) ;
#3229 = EDGE_CURVE ( 'NONE', #2164, #4508, #7390, .T. ) ;
#3230 = DIRECTION ( 'NONE',  ( 0.000000000000000000, 0.8660254037844381525, -0.5000000000000009992 ) ) ;
#3231 = CARTESIAN_POINT ( 'NONE',  ( 41.95042219981620235, 87.04630884801559887, 1.280157006458500613 ) ) ;
#3232 = CARTESIAN_POINT ( 'NONE',  ( -2.000000000000022649, -3.464101615137742396, 0.000000000000000000 ) ) ;
#3233 = AXIS2_PLACEMENT_3D ( 'NONE', #486, #2452, #3024 ) ;
#3234 = APPLICATION_CONTEXT ( 'automotive_design' ) ;
#3235 = ORIENTED_EDGE ( 'NONE', *, *, #1298, .T. ) ;
#3236 = ADVANCED_FACE ( 'NONE', ( #4515 ), #1359, .F. ) ;
#3237 = DIRECTION ( 'NONE',  ( 0.000000000000000000, 0.000000000000000000, 1.000000000000000000 ) ) ;
#3238 = DIRECTION ( 'NONE',  ( 1.000000000000000000, 0.000000000000000000, 0.000000000000000000 ) ) ;
#3239 = CARTESIAN_POINT ( 'NONE',  ( 5.000000000000015099, 0.000000000000000000, 4.250000000000000000 ) ) ;
#3240 = CARTESIAN_POINT ( 'NONE',  ( -49.94601516505092320, 87.32303837806215085, -0.6228612347031499130 ) ) ;
#3241 = ORIENTED_EDGE ( 'NONE', *, *, #3907, .T. ) ;
#3242 = EDGE_CURVE ( 'NONE', #4815, #1263, #3832, .T. ) ;
#3243 = DIRECTION ( 'NONE',  ( 0.000000000000000000, 0.000000000000000000, 1.000000000000000000 ) ) ;
#3244 = CARTESIAN_POINT ( 'NONE',  ( 1.300000000000000044, 1.478016689125442484, -1.626303258728256651E-15 ) ) ;
#3245 = LINE ( 'NONE', #1961, #3820 ) ;
#3246 = B_SPLINE_CURVE_WITH_KNOTS ( 'NONE', 3,
 ( #3752, #488, #4410, #7517 ),
 .UNSPECIFIED., .F., .F.,
 ( 4, 4 ),
 ( 2.380737581781827115E-07, 0.002336974151641521731 ),
 .UNSPECIFIED. ) ;
#3247 = CARTESIAN_POINT ( 'NONE',  ( -0.3263565795980845063, 4.430380094434251070, -2.451519936624993345 ) ) ;
#3248 = CARTESIAN_POINT ( 'NONE',  ( -49.96742166427387843, 83.19195211451609850, 1.586024383261720239 ) ) ;
#3249 = VERTEX_POINT ( 'NONE', #7371 ) ;
#3250 =( GEOMETRIC_REPRESENTATION_CONTEXT ( 3 ) GLOBAL_UNCERTAINTY_ASSIGNED_CONTEXT ( ( #3999 ) ) GLOBAL_UNIT_ASSIGNED_CONTEXT ( ( #7707, #140, #868 ) ) REPRESENTATION_CONTEXT ( 'NONE', 'WORKASPACE' ) );
#3251 = ORIENTED_EDGE ( 'NONE', *, *, #1277, .T. ) ;
#3252 = CARTESIAN_POINT ( 'NONE',  ( 41.99613340007108064, 84.41915023570773258, 2.331601159595727779 ) ) ;
#3253 = ORIENTED_EDGE ( 'NONE', *, *, #1634, .T. ) ;
#3254 = ORIENTED_EDGE ( 'NONE', *, *, #7110, .T. ) ;
#3255 = CARTESIAN_POINT ( 'NONE',  ( -4.999999999999993783, 0.000000000000000000, 5.400000000000002132 ) ) ;
#3256 = CONICAL_SURFACE ( 'NONE', #2455, 1.610000000000000098, 0.7853981633974647103 ) ;
#3257 = DIRECTION ( 'NONE',  ( 0.000000000000000000, 1.000000000000000000, -1.100686371591861952E-15 ) ) ;
#3258 = PLANE ( 'NONE',  #3975 ) ;
#3259 = DIRECTION ( 'NONE',  ( -4.190029316300689632E-17, 6.656874088836135612E-17, 1.000000000000000000 ) ) ;
#3260 = ORIENTED_EDGE ( 'NONE', *, *, #7203, .T. ) ;
#3261 = PRODUCT_RELATED_PRODUCT_CATEGORY ( 'part', '', ( #1201 ) ) ;
#3262 = ORIENTED_EDGE ( 'NONE', *, *, #6255, .T. ) ;
#3263 = ADVANCED_FACE ( 'NONE', ( #3730 ), #558, .F. ) ;
#3264 = ADVANCED_FACE ( 'NONE', ( #1227 ), #6068, .F. ) ;
#3265 = ORIENTED_EDGE ( 'NONE', *, *, #7559, .T. ) ;
#3266 = CARTESIAN_POINT ( 'NONE',  ( 30.00000000000000000, 2.516649172247811061E-16, -2.055000000000006821 ) ) ;
#3267 = CARTESIAN_POINT ( 'NONE',  ( 41.93355926540186118, 82.63845406065466648, -0.4466446237676945930 ) ) ;
#3268 = CARTESIAN_POINT ( 'NONE',  ( 2.500000000000002220, 3.061616997868386099E-16, -2.674599999999998978 ) ) ;
#3269 = CARTESIAN_POINT ( 'NONE',  ( 2.650000000000003020, 3.245314017740489906E-16, 10.00000000000000000 ) ) ;
#3270 =( NAMED_UNIT ( * ) SI_UNIT ( $, .STERADIAN. ) SOLID_ANGLE_UNIT ( ) );
#3271 = CARTESIAN_POINT ( 'NONE',  ( -34.99999999999999289, 30.00000000000000711, 10.00000000000000000 ) ) ;
#3272 = ADVANCED_FACE ( 'NONE', ( #5946 ), #4878, .T. ) ;
#3273 = FACE_OUTER_BOUND ( 'NONE', #4969, .T. ) ;
#3274 = CYLINDRICAL_SURFACE ( 'NONE', #562, 2.650000000000002576 ) ;
#3275 = EDGE_CURVE ( 'NONE', #4032, #4428, #250, .T. ) ;
#3276 = AXIS2_PLACEMENT_3D ( 'NONE', #8110, #2427, #6952 ) ;
#3277 = ORIENTED_EDGE ( 'NONE', *, *, #1212, .F. ) ;
#3278 = CARTESIAN_POINT ( 'NONE',  ( -31.74999999999995737, 2.449293598294707893E-16, -2.000000000000000888 ) ) ;
#3279 = DIRECTION ( 'NONE',  ( -1.000000000000000000, 0.000000000000000000, 0.000000000000000000 ) ) ;
#3280 = FACE_OUTER_BOUND ( 'NONE', #3603, .T. ) ;
#3281 = CARTESIAN_POINT ( 'NONE',  ( 0.000000000000000000, 0.000000000000000000, 0.000000000000000000 ) ) ;
#3282 = DIRECTION ( 'NONE',  ( 1.000000000000000000, -0.000000000000000000, -0.000000000000000000 ) ) ;
#3283 = ORIENTED_EDGE ( 'NONE', *, *, #3460, .T. ) ;
#3284 = ORIENTED_EDGE ( 'NONE', *, *, #4538, .F. ) ;
#3285 = CARTESIAN_POINT ( 'NONE',  ( -60.00000000000000000, 10.00000000000000000, 10.50000000000000000 ) ) ;
#3286 = VERTEX_POINT ( 'NONE', #4667 ) ;
#3287 = VERTEX_POINT ( 'NONE', #2750 ) ;
#3288 = CARTESIAN_POINT ( 'NONE',  ( -39.83716857408418122, 108.0000000000001990, -4.999999999999976907 ) ) ;
#3289 = DIRECTION ( 'NONE',  ( -0.000000000000000000, -0.000000000000000000, 1.000000000000000000 ) ) ;
#3290 = CARTESIAN_POINT ( 'NONE',  ( 32.64999999999997726, 30.00000000000001421, 1.734723475976807094E-15 ) ) ;
#3291 = DIRECTION ( 'NONE',  ( -2.542445703451683077E-18, -3.122502256758271259E-17, -1.000000000000000000 ) ) ;
#3292 = EDGE_CURVE ( 'NONE', #8100, #3918, #6492, .T. ) ;
#3293 = AXIS2_PLACEMENT_3D ( 'NONE', #3097, #5639, #8153 ) ;
#3294 = EDGE_CURVE ( 'NONE', #1037, #2831, #7231, .T. ) ;
#3295 =( GEOMETRIC_REPRESENTATION_CONTEXT ( 3 ) GLOBAL_UNCERTAINTY_ASSIGNED_CONTEXT ( ( #4292 ) ) GLOBAL_UNIT_ASSIGNED_CONTEXT ( ( #2347, #3822, #3270 ) ) REPRESENTATION_CONTEXT ( 'NONE', 'WORKASPACE' ) );
#3296 = VERTEX_POINT ( 'NONE', #4046 ) ;
#3297 = VERTEX_POINT ( 'NONE', #832 ) ;
#3298 = ORIENTED_EDGE ( 'NONE', *, *, #3541, .F. ) ;
#3299 = AXIS2_PLACEMENT_3D ( 'NONE', #3577, #7436, #4118 ) ;
#3300 = CARTESIAN_POINT ( 'NONE',  ( -50.00000000000000711, 85.00000000000009948, -2.399999999999999467 ) ) ;
#3301 = CARTESIAN_POINT ( 'NONE',  ( 41.97210380486419723, 86.53394040609762783, -1.850206309318216169 ) ) ;
#3302 = DIRECTION ( 'NONE',  ( -1.000000000000000000, 0.000000000000000000, 1.412205397084726379E-17 ) ) ;
#3303 = AXIS2_PLACEMENT_3D ( 'NONE', #4059, #2695, #186 ) ;
#3304 = CIRCLE ( 'NONE', #501, 1.535500000000000087 ) ;
#3305 = VERTEX_POINT ( 'NONE', #173 ) ;
#3306 =( LENGTH_UNIT ( ) NAMED_UNIT ( * ) SI_UNIT ( .MILLI., .METRE. ) );
#3307 = CONICAL_SURFACE ( 'NONE', #1574, 1.280000000000000027, 1.047197551196593857 ) ;
#3308 = AXIS2_PLACEMENT_3D ( 'NONE', #1992, #4523, #7049 ) ;
#3309 = CIRCLE ( 'NONE', #3571, 3.299999999999999822 ) ;
#3310 = CIRCLE ( 'NONE', #3187, 4.999999999999997335 ) ;
#3311 = VECTOR ( 'NONE', #3692, 1000.000000000000000 ) ;
#3312 = DIRECTION ( 'NONE',  ( 1.000000000000000000, 0.000000000000000000, 0.000000000000000000 ) ) ;
#3313 = ADVANCED_FACE ( 'NONE', ( #2093 ), #4554, .F. ) ;
#3314 = DIRECTION ( 'NONE',  ( -1.000000000000000000, 0.000000000000000000, 0.000000000000000000 ) ) ;
#3315 = DIRECTION ( 'NONE',  ( -1.412205397084881070E-17, 2.775557561562891967E-17, 1.000000000000000000 ) ) ;
#3316 = EDGE_CURVE ( 'NONE', #7075, #5556, #1398, .T. ) ;
#3317 =( REPRESENTATION_RELATIONSHIP ('NONE','NONE', #3916, #7239 ) REPRESENTATION_RELATIONSHIP_WITH_TRANSFORMATION ( #7481 )SHAPE_REPRESENTATION_RELATIONSHIP( ) );
#3318 = CIRCLE ( 'NONE', #2118, 2.650000000000003020 ) ;
#3319 = FACE_OUTER_BOUND ( 'NONE', #506, .T. ) ;
#3320 = DIRECTION ( 'NONE',  ( 0.000000000000000000, 0.000000000000000000, 1.000000000000000000 ) ) ;
#3321 = AXIS2_PLACEMENT_3D ( 'NONE', #8034, #3070, #6797 ) ;
#3322 = ADVANCED_FACE ( 'NONE', ( #5337 ), #5258, .T. ) ;
#3323 = ORIENTED_EDGE ( 'NONE', *, *, #6084, .T. ) ;
#3324 = CIRCLE ( 'NONE', #4386, 1.250000000000001110 ) ;
#3325 = FACE_OUTER_BOUND ( 'NONE', #4284, .T. ) ;
#3326 = AXIS2_PLACEMENT_3D ( 'NONE', #6531, #6077, #841 ) ;
#3327 = FACE_OUTER_BOUND ( 'NONE', #619, .T. ) ;
#3328 = FACE_OUTER_BOUND ( 'NONE', #4863, .T. ) ;
#3329 = EDGE_CURVE ( 'NONE', #5320, #1740, #3378, .T. ) ;
#3330 = CARTESIAN_POINT ( 'NONE',  ( 2.000000000000000000, 0.000000000000000000, 1.535500000000000087 ) ) ;
#3331 = ORIENTED_EDGE ( 'NONE', *, *, #241, .F. ) ;
#3332 = DIRECTION ( 'NONE',  ( -1.000000000000000000, 0.000000000000000000, 0.000000000000000000 ) ) ;
#3333 = AXIS2_PLACEMENT_3D ( 'NONE', #6627, #2312, #393 ) ;
#3334 = ORIENTED_EDGE ( 'NONE', *, *, #5059, .F. ) ;
#3335 = ORIENTED_EDGE ( 'NONE', *, *, #1556, .T. ) ;
#3336 = ORIENTED_EDGE ( 'NONE', *, *, #7984, .T. ) ;
#3337 = VERTEX_POINT ( 'NONE', #4015 ) ;
#3338 = DIRECTION ( 'NONE',  ( 1.000000000000000000, 0.000000000000000000, 0.000000000000000000 ) ) ;
#3339 = CARTESIAN_POINT ( 'NONE',  ( 1.270137496355039850E-14, 85.00000000000011369, 5.000000000000046185 ) ) ;
#3340 = DIRECTION ( 'NONE',  ( 3.351310466624018316E-17, -3.122502256758225653E-17, -1.000000000000000000 ) ) ;
#3341 = ORIENTED_EDGE ( 'NONE', *, *, #5153, .F. ) ;
#3342 = ORIENTED_EDGE ( 'NONE', *, *, #2839, .T. ) ;
#3343 = ORIENTED_EDGE ( 'NONE', *, *, #7645, .F. ) ;
#3344 = DIRECTION ( 'NONE',  ( -1.000000000000000000, 0.000000000000000000, 1.112002228190260397E-17 ) ) ;
#3345 = DIRECTION ( 'NONE',  ( 0.000000000000000000, -1.224646799147353207E-16, 1.000000000000000000 ) ) ;
#3346 = LINE ( 'NONE', #5873, #2351 ) ;
#3347 = EDGE_CURVE ( 'NONE', #135, #7449, #1433, .T. ) ;
#3348 = AXIS2_PLACEMENT_3D ( 'NONE', #4281, #7433, #6806 ) ;
#3349 = FACE_OUTER_BOUND ( 'NONE', #7195, .T. ) ;
#3350 = FACE_OUTER_BOUND ( 'NONE', #6063, .T. ) ;
#3351 = CARTESIAN_POINT ( 'NONE',  ( -7.000000000000000000, 0.000000000000000000, 18.00000000000000355 ) ) ;
#3352 = CARTESIAN_POINT ( 'NONE',  ( 58.00000000000000000, -8.000000000000000000, -8.000000000000000000 ) ) ;
#3353 = AXIS2_PLACEMENT_3D ( 'NONE', #5681, #2774, #2152 ) ;
#3354 = EDGE_CURVE ( 'NONE', #2847, #3149, #6586, .T. ) ;
#3355 = EDGE_CURVE ( 'NONE', #3305, #5664, #3968, .T. ) ;
#3356 = ORIENTED_EDGE ( 'NONE', *, *, #5203, .T. ) ;
#3357 = ADVANCED_FACE ( 'NONE', ( #3416 ), #6733, .F. ) ;
#3358 = CARTESIAN_POINT ( 'NONE',  ( 60.00000000000000711, -10.00000000000000000, 60.00000000000000000 ) ) ;
#3359 = DIRECTION ( 'NONE',  ( 1.000000000000000000, 0.000000000000000000, 0.000000000000000000 ) ) ;
#3360 = ADVANCED_FACE ( 'NONE', ( #204 ), #7256, .T. ) ;
#3361 = PLANE ( 'NONE',  #7377 ) ;
#3362 = CARTESIAN_POINT ( 'NONE',  ( 1.270137496355039850E-14, 85.00000000000011369, 5.000000000000046185 ) ) ;
#3363 = DIRECTION ( 'NONE',  ( -1.000000000000000000, 0.000000000000000000, 0.000000000000000000 ) ) ;
#3364 = VERTEX_POINT ( 'NONE', #2169 ) ;
#3365 = CARTESIAN_POINT ( 'NONE',  ( 50.00000000000004974, 85.00000000000039790, -2.399999999999999467 ) ) ;
#3366 = VERTEX_POINT ( 'NONE', #5838 ) ;
#3367 = EDGE_LOOP ( 'NONE', ( #3566, #7556, #1588, #2833 ) ) ;
#3368 = LINE ( 'NONE', #193, #775 ) ;
#3369 = LINE ( 'NONE', #3958, #4896 ) ;
#3370 = FACE_OUTER_BOUND ( 'NONE', #6792, .T. ) ;
#3371 = ORIENTED_EDGE ( 'NONE', *, *, #3787, .T. ) ;
#3372 = EDGE_CURVE ( 'NONE', #5731, #4177, #1024, .T. ) ;
#3373 = ORIENTED_EDGE ( 'NONE', *, *, #4682, .F. ) ;
#3374 = ORIENTED_EDGE ( 'NONE', *, *, #7329, .F. ) ;
#3375 = VECTOR ( 'NONE', #2220, 1000.000000000000227 ) ;
#3376 = CARTESIAN_POINT ( 'NONE',  ( -52.00000000000006395, -8.000000000000001776, 20.00000000000000355 ) ) ;
#3377 = CARTESIAN_POINT ( 'NONE',  ( 3.099070612933924274, -6.280812701381221608, 8.006629596177415209 ) ) ;
#3378 = LINE ( 'NONE', #3465, #1555 ) ;
#3379 = EDGE_CURVE ( 'NONE', #1461, #7794, #3346, .T. ) ;
#3380 = CARTESIAN_POINT ( 'NONE',  ( 0.000000000000000000, 0.000000000000000000, 5.400000000000002132 ) ) ;
#3381 = FACE_OUTER_BOUND ( 'NONE', #5683, .T. ) ;
#3382 = DIRECTION ( 'NONE',  ( 0.000000000000000000, 0.000000000000000000, 1.000000000000000000 ) ) ;
#3383 = CARTESIAN_POINT ( 'NONE',  ( 1.284259550325887758E-14, 85.00000000000005684, -5.000000000000004441 ) ) ;
#3384 = FACE_BOUND ( 'NONE', #7180, .T. ) ;
#3385 = ADVANCED_FACE ( 'NONE', ( #3627 ), #2376, .F. ) ;
#3386 = CARTESIAN_POINT ( 'NONE',  ( -60.00000000000000000, 10.00000000000000000, 20.00000000000000355 ) ) ;
#3387 = ADVANCED_FACE ( 'NONE', ( #5414 ), #4740, .T. ) ;
#3388 = VERTEX_POINT ( 'NONE', #4252 ) ;
#3389 = DIRECTION ( 'NONE',  ( 0.5000000000000026645, -0.8660254037844372643, 0.000000000000000000 ) ) ;
#3390 = CARTESIAN_POINT ( 'NONE',  ( 0.2500000000000002220, 5.204748896376238866E-16, -4.249999999999979572 ) ) ;
#3391 = FACE_OUTER_BOUND ( 'NONE', #4293, .T. ) ;
#3392 = B_SPLINE_CURVE_WITH_KNOTS ( 'NONE', 3,
 ( #2311, #1103, #4139, #6090, #5392, #3479, #5435, #392, #6003, #2973, #935, #4181, #6754, #2937, #306, #5479, #3518, #2813, #6669, #977, #2348, #4102, #7246, #1016 ),
 .UNSPECIFIED., .F., .F.,
 ( 4, 2, 2, 2, 2, 2, 2, 2, 2, 2, 2, 4 ),
 ( 0.006106748147955515411, 0.006869861680660345471, 0.007632975213365174663, 0.008396088746070003855, 0.009159202278774834782, 0.009540759045127248511, 0.009922315811479663974, 0.01030387257783207944, 0.01068542934418449317, 0.01106698611053690863, 0.01144854287688932409, 0.01221165640959417757 ),
 .UNSPECIFIED. ) ;
#3393 = CARTESIAN_POINT ( 'NONE',  ( 2.999999999999999112, 45.09008114612887397, 0.000000000000000000 ) ) ;
#3394 = CARTESIAN_POINT ( 'NONE',  ( 0.000000000000000000, 0.000000000000000000, 10.00000000000000000 ) ) ;
#3395 = DIRECTION ( 'NONE',  ( 0.000000000000000000, 0.000000000000000000, -1.000000000000000000 ) ) ;
#3396 = ORIENTED_EDGE ( 'NONE', *, *, #904, .F. ) ;
#3397 = DIRECTION ( 'NONE',  ( -0.5000000000000061062, 1.060575238724902601E-16, -0.8660254037844351549 ) ) ;
#3398 = VECTOR ( 'NONE', #6247, 1000.000000000000000 ) ;
#3399 = UNCERTAINTY_MEASURE_WITH_UNIT (LENGTH_MEASURE( 1.000000000000000082E-05 ), #2019, 'distance_accuracy_value', 'NONE');
#3400 = ORIENTED_EDGE ( 'NONE', *, *, #6998, .F. ) ;
#3401 = EDGE_LOOP ( 'NONE', ( #5943, #7911, #4628, #49, #1660 ) ) ;
#3402 = DIRECTION ( 'NONE',  ( -0.000000000000000000, -0.000000000000000000, 1.000000000000000000 ) ) ;
#3403 = AXIS2_PLACEMENT_3D ( 'NONE', #6507, #4486, #7720 ) ;
#3404 = CIRCLE ( 'NONE', #4601, 4.999999999999993783 ) ;
#3405 = DIRECTION ( 'NONE',  ( -1.000000000000000000, 0.000000000000000000, 0.000000000000000000 ) ) ;
#3406 = ADVANCED_FACE ( 'NONE', ( #2257 ), #458, .F. ) ;
#3407 = FACE_OUTER_BOUND ( 'NONE', #4700, .T. ) ;
#3408 = PRODUCT_CONTEXT ( 'NONE', #4223, 'mechanical' ) ;
#3409 = ADVANCED_FACE ( 'NONE', ( #6694 ), #2919, .F. ) ;
#3410 = ORIENTED_EDGE ( 'NONE', *, *, #2096, .T. ) ;
#3411 = ORIENTED_EDGE ( 'NONE', *, *, #6816, .F. ) ;
#3412 = ORIENTED_EDGE ( 'NONE', *, *, #4924, .T. ) ;
#3413 = EDGE_CURVE ( 'NONE', #1727, #7382, #3014, .T. ) ;
#3414 = CARTESIAN_POINT ( 'NONE',  ( 0.000000000000000000, 1.178949249685212086, -2.042000000000002036 ) ) ;
#3415 = CARTESIAN_POINT ( 'NONE',  ( -41.99800142710427764, 85.46750262719235991, 2.365737336732676610 ) ) ;
#3416 = FACE_OUTER_BOUND ( 'NONE', #5623, .T. ) ;
#3417 = AXIS2_PLACEMENT_3D ( 'NONE', #370, #6067, #6731 ) ;
#3418 =( NAMED_UNIT ( * ) PLANE_ANGLE_UNIT ( ) SI_UNIT ( $, .RADIAN. ) );
#3419 = CIRCLE ( 'NONE', #1160, 2.500000000000002220 ) ;
#3420 = FACE_OUTER_BOUND ( 'NONE', #2554, .T. ) ;
#3421 = B_SPLINE_CURVE_WITH_KNOTS ( 'NONE', 3,
 ( #5209, #5243, #1963, #6399, #7099, #7175, #4607, #4030, #703, #3248, #4224, #2149, #979, #6045, #5482, #6756, #308, #2894, #3520, #4721, #2853, #7871, #5394, #2226, #7836, #1065, #3442, #1654, #4141, #7300, #4061, #7957 ),
 .UNSPECIFIED., .F., .F.,
 ( 4, 2, 2, 2, 2, 2, 2, 2, 2, 2, 2, 2, 2, 2, 2, 4 ),
 ( 0.000000000000000000, 0.0004690358444887973298, 0.0009380716889775946596, 0.001407107533466392044, 0.001876143377955189319, 0.002345179222443986595, 0.002814215066932784087, 0.003752286755910362159, 0.004221322600399150977, 0.004690358444887940230, 0.005159394289376728615, 0.005628430133865517868, 0.006097465978354307120, 0.006566501822843097240, 0.007035537667331886492, 0.007504573511820675745 ),
 .UNSPECIFIED. ) ;
#3422 = AXIS2_PLACEMENT_3D ( 'NONE', #5619, #5856, #154 ) ;
#3423 = CYLINDRICAL_SURFACE ( 'NONE', #2111, 1.649999999999991696 ) ;
#3424 = CARTESIAN_POINT ( 'NONE',  ( 0.1999999999999987899, 4.286263797015736595E-16, -3.500000000000000000 ) ) ;
#3425 = PRESENTATION_STYLE_ASSIGNMENT (( #2140 ) ) ;
#3426 = AXIS2_PLACEMENT_3D ( 'NONE', #6193, #4291, #5539 ) ;
#3427 = CARTESIAN_POINT ( 'NONE',  ( -0.6543461111163948463, -4.241015250120822699, -0.1391502195351549120 ) ) ;
#3428 = CLOSED_SHELL ( 'NONE', ( #5877, #3236, #6109, #8157, #5270, #1416, #8108, #5444, #3357, #6644, #3515, #5076, #3441, #5200, #1070, #3850, #2457, #7977, #7969, #1270, #2389, #1566, #3812, #7082, #1340, #1553, #1098, #419 ) ) ;
#3429 = VECTOR ( 'NONE', #59, 1000.000000000000000 ) ;
#3430 = CARTESIAN_POINT ( 'NONE',  ( 0.000000000000000000, 0.000000000000000000, 3.469446951953614189E-15 ) ) ;
#3431 = CIRCLE ( 'NONE', #763, 2.649999999999995914 ) ;
#3432 = VERTEX_POINT ( 'NONE', #1041 ) ;
#3433 = PLANE ( 'NONE',  #2596 ) ;
#3434 = PLANE ( 'NONE',  #4351 ) ;
#3435 = CARTESIAN_POINT ( 'NONE',  ( 20.00000000000000355, 0.000000000000000000, 0.000000000000000000 ) ) ;
#3436 = CIRCLE ( 'NONE', #8072, 1.249999999999998002 ) ;
#3437 = VECTOR ( 'NONE', #8133, 1000.000000000000227 ) ;
#3438 = DIRECTION ( 'NONE',  ( -0.5000000000000061062, 0.000000000000000000, 0.8660254037844351549 ) ) ;
#3439 = FACE_OUTER_BOUND ( 'NONE', #5969, .T. ) ;
#3440 = AXIS2_PLACEMENT_3D ( 'NONE', #266, #2814, #7869 ) ;
#3441 = ADVANCED_FACE ( 'NONE', ( #1764 ), #7890, .T. ) ;
#3442 = CARTESIAN_POINT ( 'NONE',  ( -49.98889375043668082, 83.93620601285597616, -2.157108981641785217 ) ) ;
#3443 = EDGE_CURVE ( 'NONE', #7226, #4246, #3732, .T. ) ;
#3444 = FACE_OUTER_BOUND ( 'NONE', #4457, .T. ) ;
#3445 = ORIENTED_EDGE ( 'NONE', *, *, #3937, .F. ) ;
#3446 = CIRCLE ( 'NONE', #1726, 39.00000000000002132 ) ;
#3447 = DIRECTION ( 'NONE',  ( -1.000000000000000000, -0.000000000000000000, -0.000000000000000000 ) ) ;
#3448 = TOROIDAL_SURFACE ( 'NONE', #8081, 1.600000000000000311, 0.1000000000000000056 ) ;
#3449 = ORIENTED_EDGE ( 'NONE', *, *, #1469, .T. ) ;
#3450 = AXIS2_PLACEMENT_3D ( 'NONE', #4170, #7326, #210 ) ;
#3451 = ORIENTED_EDGE ( 'NONE', *, *, #7776, .T. ) ;
#3452 =( GEOMETRIC_REPRESENTATION_CONTEXT ( 3 ) GLOBAL_UNCERTAINTY_ASSIGNED_CONTEXT ( ( #7365 ) ) GLOBAL_UNIT_ASSIGNED_CONTEXT ( ( #5891, #7683, #70 ) ) REPRESENTATION_CONTEXT ( 'NONE', 'WORKASPACE' ) );
#3453 = DIRECTION ( 'NONE',  ( 0.000000000000000000, 1.000000000000000000, 0.000000000000000000 ) ) ;
#3454 = CARTESIAN_POINT ( 'NONE',  ( 4.000000000000003553, 0.3904826640788058856, -2.699999999999998401 ) ) ;
#3455 = FACE_OUTER_BOUND ( 'NONE', #3123, .T. ) ;
#3456 = FACE_OUTER_BOUND ( 'NONE', #4185, .T. ) ;
#3457 = PRODUCT_CONTEXT ( 'NONE', #3487, 'mechanical' ) ;
#3458 = VERTEX_POINT ( 'NONE', #3590 ) ;
#3459 = EDGE_CURVE ( 'NONE', #135, #953, #2208, .T. ) ;
#3460 = EDGE_CURVE ( 'NONE', #8184, #4662, #7976, .T. ) ;
#3461 = ORIENTED_EDGE ( 'NONE', *, *, #2458, .F. ) ;
#3462 = VERTEX_POINT ( 'NONE', #4739 ) ;
#3463 = CARTESIAN_POINT ( 'NONE',  ( 1.270137496355039850E-14, 85.00000000000011369, 5.000000000000046185 ) ) ;
#3464 = CARTESIAN_POINT ( 'NONE',  ( -41.97904239022133055, 86.32664991614245764, 2.000000000000043521 ) ) ;
#3465 = CARTESIAN_POINT ( 'NONE',  ( 11.00000000000000355, 1.493456771560197319E-16, -1.219500000000000028 ) ) ;
#3466 = VECTOR ( 'NONE', #2342, 1000.000000000000114 ) ;
#3467 =( LENGTH_UNIT ( ) NAMED_UNIT ( * ) SI_UNIT ( .MILLI., .METRE. ) );
#3468 = CARTESIAN_POINT ( 'NONE',  ( 0.000000000000000000, 0.000000000000000000, 0.000000000000000000 ) ) ;
#3469 = CARTESIAN_POINT ( 'NONE',  ( -30.00000000000000355, -29.99999999999999289, 10.00000000000000000 ) ) ;
#3470 = CARTESIAN_POINT ( 'NONE',  ( 3.000000000000000888, 2.750000000000000000, 0.000000000000000000 ) ) ;
#3471 = DIRECTION ( 'NONE',  ( -1.000000000000000000, 0.000000000000000000, -0.000000000000000000 ) ) ;
#3472 = CIRCLE ( 'NONE', #6267, 2.500000000000000444 ) ;
#3473 = EDGE_CURVE ( 'NONE', #6062, #2593, #2664, .T. ) ;
#3474 = ORIENTED_EDGE ( 'NONE', *, *, #7782, .F. ) ;
#3475 = ORIENTED_EDGE ( 'NONE', *, *, #6818, .F. ) ;
#3476 = DIRECTION ( 'NONE',  ( 0.000000000000000000, 0.000000000000000000, -1.000000000000000000 ) ) ;
#3477 = DIRECTION ( 'NONE',  ( -1.000000000000000000, 0.000000000000000000, 0.000000000000000000 ) ) ;
#3478 = CARTESIAN_POINT ( 'NONE',  ( 0.000000000000000000, 0.000000000000000000, 0.000000000000000000 ) ) ;
#3479 = CARTESIAN_POINT ( 'NONE',  ( -41.96864087686231670, 86.63551061574989376, -1.774759388940247984 ) ) ;
#3480 = CARTESIAN_POINT ( 'NONE',  ( 60.00000000000000711, -10.00000000000000000, 19.99999999999998224 ) ) ;
#3481 = FACE_OUTER_BOUND ( 'NONE', #2345, .T. ) ;
#3482 = AXIS2_PLACEMENT_3D ( 'NONE', #4434, #7594, #1232 ) ;
#3483 = DIRECTION ( 'NONE',  ( -1.000000000000000000, 0.000000000000000000, 0.000000000000000000 ) ) ;
#3484 = ORIENTED_EDGE ( 'NONE', *, *, #4027, .T. ) ;
#3485 = CARTESIAN_POINT ( 'NONE',  ( 60.00000000000000711, 10.00000000000000000, 60.00000000000000000 ) ) ;
#3486 = ORIENTED_EDGE ( 'NONE', *, *, #1117, .F. ) ;
#3487 = APPLICATION_CONTEXT ( 'automotive_design' ) ;
#3488 = EDGE_LOOP ( 'NONE', ( #3374, #3640, #3996, #5251 ) ) ;
#3489 = DIRECTION ( 'NONE',  ( 1.000000000000000000, 0.000000000000000000, 0.000000000000000000 ) ) ;
#3490 = PLANE ( 'NONE',  #510 ) ;
#3491 = CARTESIAN_POINT ( 'NONE',  ( 4.000000000000003553, -0.3902508023145564442, -2.699999999999998845 ) ) ;
#3492 = CARTESIAN_POINT ( 'NONE',  ( -25.00000000000000711, -29.99999999999999289, 10.00000000000000000 ) ) ;
#3493 = DIRECTION ( 'NONE',  ( 0.000000000000000000, 0.000000000000000000, 1.000000000000000000 ) ) ;
#3494 = APPLICATION_PROTOCOL_DEFINITION ( 'draft international standard', 'automotive_design', 1998, #7736 ) ;
#3495 = VERTEX_POINT ( 'NONE', #7397 ) ;
#3496 = ADVANCED_FACE ( 'NONE', ( #4126, #2297, #7273 ), #1597, .T. ) ;
#3497 = ORIENTED_EDGE ( 'NONE', *, *, #6688, .T. ) ;
#3498 = ORIENTED_EDGE ( 'NONE', *, *, #5637, .F. ) ;
#3499 = CARTESIAN_POINT ( 'NONE',  ( 0.000000000000000000, 0.000000000000000000, 0.000000000000000000 ) ) ;
#3500 = CARTESIAN_POINT ( 'NONE',  ( 6.280460229959847318, -3.099761751707934998, 8.027336706075139716 ) ) ;
#3501 = CYLINDRICAL_SURFACE ( 'NONE', #108, 42.00000000000002132 ) ;
#3502 = AXIS2_PLACEMENT_3D ( 'NONE', #4501, #3179, #7071 ) ;
#3503 = ORIENTED_EDGE ( 'NONE', *, *, #1298, .F. ) ;
#3504 = PLANE ( 'NONE',  #7518 ) ;
#3505 =( GEOMETRIC_REPRESENTATION_CONTEXT ( 3 ) GLOBAL_UNCERTAINTY_ASSIGNED_CONTEXT ( ( #3399 ) ) GLOBAL_UNIT_ASSIGNED_CONTEXT ( ( #2019, #1391, #1937 ) ) REPRESENTATION_CONTEXT ( 'NONE', 'WORKASPACE' ) );
#3506 = DIRECTION ( 'NONE',  ( -0.000000000000000000, -0.000000000000000000, -1.000000000000000000 ) ) ;
#3507 = DIRECTION ( 'NONE',  ( -1.000000000000000000, -0.000000000000000000, -0.000000000000000000 ) ) ;
#3508 =( NAMED_UNIT ( * ) SI_UNIT ( $, .STERADIAN. ) SOLID_ANGLE_UNIT ( ) );
#3509 = AXIS2_PLACEMENT_3D ( 'NONE', #2580, #5775, #7558 ) ;
#3510 = LINE ( 'NONE', #3351, #4259 ) ;
#3511 = CARTESIAN_POINT ( 'NONE',  ( 1.300000000000000044, 0.000000000000000000, 0.000000000000000000 ) ) ;
#3512 = ORIENTED_EDGE ( 'NONE', *, *, #398, .F. ) ;
#3513 = ORIENTED_EDGE ( 'NONE', *, *, #6630, .F. ) ;
#3514 = CARTESIAN_POINT ( 'NONE',  ( 3.000000000000000888, 0.000000000000000000, 0.000000000000000000 ) ) ;
#3515 = ADVANCED_FACE ( 'NONE', ( #958 ), #3501, .F. ) ;
#3516 = CARTESIAN_POINT ( 'NONE',  ( 4.000000000000003553, 2.309401076758524685, -2.342734410091827701 ) ) ;
#3517 = DIRECTION ( 'NONE',  ( -0.000000000000000000, -0.000000000000000000, -1.000000000000000000 ) ) ;
#3518 = CARTESIAN_POINT ( 'NONE',  ( -41.93694813901188212, 87.30092581718484723, 0.6942729367013813491 ) ) ;
#3519 = CYLINDRICAL_SURFACE ( 'NONE', #5828, 2.649999999999995914 ) ;
#3520 = CARTESIAN_POINT ( 'NONE',  ( -49.94812488057640110, 82.72218486298729090, -0.7721950313463720184 ) ) ;
#3521 = CYLINDRICAL_SURFACE ( 'NONE', #7978, 2.500000000000000444 ) ;
#3522 = ORIENTED_EDGE ( 'NONE', *, *, #3974, .T. ) ;
#3523 = CARTESIAN_POINT ( 'NONE',  ( -31.74999999999995737, 0.000000000000000000, 0.000000000000000000 ) ) ;
#3524 = VERTEX_POINT ( 'NONE', #5500 ) ;
#3525 = ORIENTED_EDGE ( 'NONE', *, *, #4636, .T. ) ;
#3526 = DIRECTION ( 'NONE',  ( -0.000000000000000000, -0.000000000000000000, 1.000000000000000000 ) ) ;
#3527 = LINE ( 'NONE', #7431, #4232 ) ;
#3528 = CARTESIAN_POINT ( 'NONE',  ( 4.000000000000003553, -1.933795701539621437, -2.451162342337698252 ) ) ;
#3529 = CARTESIAN_POINT ( 'NONE',  ( 60.00000000000000711, 10.00000000000000000, 0.000000000000000000 ) ) ;
#3530 = CARTESIAN_POINT ( 'NONE',  ( -31.74999999999995737, 0.000000000000000000, 0.000000000000000000 ) ) ;
#3531 = AXIS2_PLACEMENT_3D ( 'NONE', #1725, #1088, #3632 ) ;
#3532 = APPLICATION_PROTOCOL_DEFINITION ( 'draft international standard', 'automotive_design', 1998, #3487 ) ;
#3533 = ORIENTED_EDGE ( 'NONE', *, *, #968, .F. ) ;
#3534 = EDGE_LOOP ( 'NONE', ( #3126, #4868, #2044 ) ) ;
#3535 = VECTOR ( 'NONE', #6799, 1000.000000000000000 ) ;
#3536 = ORIENTED_EDGE ( 'NONE', *, *, #3809, .T. ) ;
#3537 = FACE_OUTER_BOUND ( 'NONE', #7838, .T. ) ;
#3538 = EDGE_CURVE ( 'NONE', #580, #7574, #1127, .T. ) ;
#3539 = DIRECTION ( 'NONE',  ( 0.000000000000000000, 0.000000000000000000, -1.000000000000000000 ) ) ;
#3540 = CARTESIAN_POINT ( 'NONE',  ( 1.270137496355039850E-14, 85.00000000000011369, 5.000000000000046185 ) ) ;
#3541 = EDGE_CURVE ( 'NONE', #1678, #1738, #8016, .T. ) ;
#3542 = EDGE_CURVE ( 'NONE', #6538, #3388, #3762, .T. ) ;
#3543 = ORIENTED_EDGE ( 'NONE', *, *, #2323, .T. ) ;
#3544 = DIRECTION ( 'NONE',  ( 1.412205397084881070E-17, -2.775557561562891967E-17, -1.000000000000000000 ) ) ;
#3545 = FACE_OUTER_BOUND ( 'NONE', #1838, .T. ) ;
#3546 = CARTESIAN_POINT ( 'NONE',  ( 5.000000000000018652, 0.000000000000000000, -2.700000000000004174 ) ) ;
#3547 = SURFACE_SIDE_STYLE ('',( #7364 ) ) ;
#3548 = UNCERTAINTY_MEASURE_WITH_UNIT (LENGTH_MEASURE( 1.000000000000000082E-05 ), #3306, 'distance_accuracy_value', 'NONE');
#3549 = DIRECTION ( 'NONE',  ( 0.000000000000000000, -0.000000000000000000, -1.000000000000000000 ) ) ;
#3550 = AXIS2_PLACEMENT_3D ( 'NONE', #3933, #751, #2133 ) ;
#3551 = VECTOR ( 'NONE', #1562, 1000.000000000000000 ) ;
#3552 = EDGE_CURVE ( 'NONE', #493, #1081, #8144, .T. ) ;
#3553 = VERTEX_POINT ( 'NONE', #3884 ) ;
#3554 = ORIENTED_EDGE ( 'NONE', *, *, #2262, .F. ) ;
#3555 = CIRCLE ( 'NONE', #1032, 2.149999999999995470 ) ;
#3556 = CARTESIAN_POINT ( 'NONE',  ( 9.020562075079396891E-14, -10.00000000000000000, 729.2499999999977263 ) ) ;
#3557 = CARTESIAN_POINT ( 'NONE',  ( 2.500000000000002220, 2.357898499370434386, -3.469446951953614189E-15 ) ) ;
#3558 = CARTESIAN_POINT ( 'NONE',  ( -4.000000000000000000, -2.309401076758531346, -0.3572655899081733644 ) ) ;
#3559 = DIRECTION ( 'NONE',  ( 0.000000000000000000, -1.224646799147353454E-16, 1.000000000000000000 ) ) ;
#3560 = DIRECTION ( 'NONE',  ( -0.000000000000000000, -0.000000000000000000, -1.000000000000000000 ) ) ;
#3561 = VECTOR ( 'NONE', #1194, 1000.000000000000000 ) ;
#3562 = LINE ( 'NONE', #6094, #7027 ) ;
#3563 = EDGE_LOOP ( 'NONE', ( #6277, #7701 ) ) ;
#3564 = DIRECTION ( 'NONE',  ( 0.000000000000000000, 0.000000000000000000, -1.000000000000000000 ) ) ;
#3565 = EDGE_CURVE ( 'NONE', #3851, #3524, #548, .T. ) ;
#3566 = ORIENTED_EDGE ( 'NONE', *, *, #253, .F. ) ;
#3567 = VECTOR ( 'NONE', #6475, 1000.000000000000114 ) ;
#3568 = ORIENTED_EDGE ( 'NONE', *, *, #4117, .F. ) ;
#3569 = VECTOR ( 'NONE', #5238, 1000.000000000000000 ) ;
#3570 = ADVANCED_FACE ( 'NONE', ( #46 ), #3088, .F. ) ;
#3571 = AXIS2_PLACEMENT_3D ( 'NONE', #3468, #803, #2098 ) ;
#3572 = DIRECTION ( 'NONE',  ( 1.000000000000000000, 0.000000000000000000, 0.000000000000000000 ) ) ;
#3573 = VECTOR ( 'NONE', #1527, 1000.000000000000000 ) ;
#3574 = CARTESIAN_POINT ( 'NONE',  ( 4.000000000000000000, 0.000000000000000000, -2.700000000000001066 ) ) ;
#3575 = DIRECTION ( 'NONE',  ( 0.000000000000000000, -1.287488025362403787E-15, -1.000000000000000000 ) ) ;
#3576 = PLANE ( 'NONE',  #8198 ) ;
#3577 = CARTESIAN_POINT ( 'NONE',  ( 1.300000000000000044, -0.7390083445627200209, 1.280000000000001137 ) ) ;
#3578 = CONTEXT_DEPENDENT_SHAPE_REPRESENTATION ( #4160, #381 ) ;
#3579 = AXIS2_PLACEMENT_3D ( 'NONE', #796, #865, #4665 ) ;
#3580 = CIRCLE ( 'NONE', #2658, 4.000000000000000888 ) ;
#3581 = ORIENTED_EDGE ( 'NONE', *, *, #5633, .F. ) ;
#3582 = ORIENTED_EDGE ( 'NONE', *, *, #5063, .F. ) ;
#3583 = EDGE_CURVE ( 'NONE', #7674, #5320, #896, .T. ) ;
#3584 = ORIENTED_EDGE ( 'NONE', *, *, #4356, .F. ) ;
#3585 = PRODUCT_DEFINITION_SHAPE ( 'NONE', 'NONE',  #7665 ) ;
#3586 = CARTESIAN_POINT ( 'NONE',  ( 2.999999999999999112, 45.09008114612887397, 0.000000000000000000 ) ) ;
#3587 = DIRECTION ( 'NONE',  ( -1.000000000000000000, 0.000000000000000000, 0.000000000000000000 ) ) ;
#3588 = CIRCLE ( 'NONE', #921, 0.2000000000000000944 ) ;
#3589 = VECTOR ( 'NONE', #607, 1000.000000000000000 ) ;
#3590 = CARTESIAN_POINT ( 'NONE',  ( 2.000000000000000000, -1.502314598737159623E-15, -1.535500000000000087 ) ) ;
#3591 = ORIENTED_EDGE ( 'NONE', *, *, #2023, .T. ) ;
#3592 = CARTESIAN_POINT ( 'NONE',  ( -4.000000000000000000, -2.309401076758525573, -2.700000000000000178 ) ) ;
#3593 = AXIS2_PLACEMENT_3D ( 'NONE', #2753, #6610, #1600 ) ;
#3594 = ORIENTED_EDGE ( 'NONE', *, *, #5740, .F. ) ;
#3595 = EDGE_CURVE ( 'NONE', #4814, #3913, #5628, .T. ) ;
#3596 = AXIS2_PLACEMENT_3D ( 'NONE', #6967, #7601, #4561 ) ;
#3597 = CARTESIAN_POINT ( 'NONE',  ( 42.00000000000003553, 85.23349283444500202, 2.399999999999973266 ) ) ;
#3598 = DIRECTION ( 'NONE',  ( -0.000000000000000000, -0.000000000000000000, 1.000000000000000000 ) ) ;
#3599 = SHAPE_REPRESENTATION_RELATIONSHIP ( 'NONE' , 'NONE' ,  #1368, #4869 ) ;
#3600 =( NAMED_UNIT ( * ) SI_UNIT ( $, .STERADIAN. ) SOLID_ANGLE_UNIT ( ) );
#3601 = CYLINDRICAL_SURFACE ( 'NONE', #161, 2.000000000000000888 ) ;
#3602 = ORIENTED_EDGE ( 'NONE', *, *, #292, .F. ) ;
#3603 = EDGE_LOOP ( 'NONE', ( #4497, #4414 ) ) ;
#3604 =( LENGTH_UNIT ( ) NAMED_UNIT ( * ) SI_UNIT ( .MILLI., .METRE. ) );
#3605 = DIRECTION ( 'NONE',  ( 0.000000000000000000, 0.000000000000000000, -1.000000000000000000 ) ) ;
#3606 = CARTESIAN_POINT ( 'NONE',  ( -60.00000000000000000, 10.00000000000000000, 20.00000000000000355 ) ) ;
#3607 = DIRECTION ( 'NONE',  ( 0.000000000000000000, -1.026972870230479989E-15, -1.000000000000000000 ) ) ;
#3608 = DIRECTION ( 'NONE',  ( 0.000000000000000000, 1.000000000000000000, -1.320393690296331133E-15 ) ) ;
#3609 = ORIENTED_EDGE ( 'NONE', *, *, #7974, .F. ) ;
#3610 = ADVANCED_FACE ( 'NONE', ( #6909 ), #3307, .F. ) ;
#3611 = DIRECTION ( 'NONE',  ( 0.000000000000000000, 0.000000000000000000, -1.000000000000000000 ) ) ;
#3612 = EDGE_CURVE ( 'NONE', #4887, #6175, #3222, .T. ) ;
#3613 = EDGE_CURVE ( 'NONE', #3962, #8142, #7676, .T. ) ;
#3614 = VERTEX_POINT ( 'NONE', #1351 ) ;
#3615 = VERTEX_POINT ( 'NONE', #2423 ) ;
#3616 = DIRECTION ( 'NONE',  ( 0.000000000000000000, 0.000000000000000000, 1.000000000000000000 ) ) ;
#3617 = CARTESIAN_POINT ( 'NONE',  ( 4.999999999999990230, 0.000000000000000000, 20.00000000000000355 ) ) ;
#3618 = CARTESIAN_POINT ( 'NONE',  ( -34.99999999999999289, -29.99999999999999289, 10.00000000000000000 ) ) ;
#3619 = AXIS2_PLACEMENT_3D ( 'NONE', #5366, #4237, #902 ) ;
#3620 = DIRECTION ( 'NONE',  ( -0.000000000000000000, -0.000000000000000000, 1.000000000000000000 ) ) ;
#3621 = LINE ( 'NONE', #7884, #642 ) ;
#3622 = EDGE_LOOP ( 'NONE', ( #5075, #6446, #3173, #625 ) ) ;
#3623 = VERTEX_POINT ( 'NONE', #3713 ) ;
#3624 = EDGE_LOOP ( 'NONE', ( #5870, #1234, #3341, #2278 ) ) ;
#3625 = FACE_BOUND ( 'NONE', #6992, .T. ) ;
#3626 = LINE ( 'NONE', #456, #5456 ) ;
#3627 = FACE_OUTER_BOUND ( 'NONE', #1828, .T. ) ;
#3628 = UNCERTAINTY_MEASURE_WITH_UNIT (LENGTH_MEASURE( 1.000000000000000082E-05 ), #6999, 'distance_accuracy_value', 'NONE');
#3629 = EDGE_CURVE ( 'NONE', #5583, #6246, #4090, .T. ) ;
#3630 = VERTEX_POINT ( 'NONE', #7580 ) ;
#3631 = ADVANCED_FACE ( 'NONE', ( #4964 ), #508, .F. ) ;
#3632 = DIRECTION ( 'NONE',  ( 0.000000000000000000, 0.000000000000000000, 1.000000000000000000 ) ) ;
#3633 = EDGE_LOOP ( 'NONE', ( #4436, #5010, #3926 ) ) ;
#3634 = EDGE_LOOP ( 'NONE', ( #1840, #6249, #1046, #748 ) ) ;
#3635 = DIRECTION ( 'NONE',  ( 1.000000000000000000, -0.000000000000000000, -0.000000000000000000 ) ) ;
#3636 = CARTESIAN_POINT ( 'NONE',  ( -41.94398068067087593, 82.82972336481591924, 1.056300034359339168 ) ) ;
#3637 = CARTESIAN_POINT ( 'NONE',  ( 0.000000000000000000, 0.000000000000000000, 0.000000000000000000 ) ) ;
#3638 = AXIS2_PLACEMENT_3D ( 'NONE', #4462, #7735, #3960 ) ;
#3639 = CARTESIAN_POINT ( 'NONE',  ( 5.948289146961254659, 3.697435614623359790, 8.024517386334258262 ) ) ;
#3640 = ORIENTED_EDGE ( 'NONE', *, *, #259, .F. ) ;
#3641 = EDGE_LOOP ( 'NONE', ( #5113, #39 ) ) ;
#3642 = AXIS2_PLACEMENT_3D ( 'NONE', #4189, #6765, #2357 ) ;
#3643 = DIRECTION ( 'NONE',  ( -0.000000000000000000, -0.000000000000000000, -1.000000000000000000 ) ) ;
#3644 = DIRECTION ( 'NONE',  ( 1.412205397084881070E-17, -2.775557561562891967E-17, -1.000000000000000000 ) ) ;
#3645 = DIRECTION ( 'NONE',  ( -1.000000000000000000, 0.000000000000000000, 0.000000000000000000 ) ) ;
#3646 = APPLICATION_CONTEXT ( 'automotive_design' ) ;
#3647 = EDGE_CURVE ( 'NONE', #4246, #3249, #6241, .T. ) ;
#3648 = DIRECTION ( 'NONE',  ( 0.000000000000000000, 0.000000000000000000, -1.000000000000000000 ) ) ;
#3649 = DIRECTION ( 'NONE',  ( -1.000000000000000000, -0.000000000000000000, -0.000000000000000000 ) ) ;
#3650 = EDGE_CURVE ( 'NONE', #1158, #6924, #4330, .T. ) ;
#3651 = DIRECTION ( 'NONE',  ( -0.000000000000000000, -0.000000000000000000, 1.000000000000000000 ) ) ;
#3652 = PRODUCT_DEFINITION_SHAPE ( 'NONE', 'NONE',  #8216 ) ;
#3653 = VERTEX_POINT ( 'NONE', #1167 ) ;
#3654 = ORIENTED_EDGE ( 'NONE', *, *, #801, .F. ) ;
#3655 = CARTESIAN_POINT ( 'NONE',  ( 0.3263565795980692408, -4.430380094434308802, -0.2484800633750388066 ) ) ;
#3656 = LINE ( 'NONE', #3075, #7932 ) ;
#3657 = DIRECTION ( 'NONE',  ( -0.7071067811865359154, 8.659560562355074607E-17, -0.7071067811865591191 ) ) ;
#3658 = FACE_OUTER_BOUND ( 'NONE', #4575, .T. ) ;
#3659 = CARTESIAN_POINT ( 'NONE',  ( -4.264990453868429121, 5.569424739774936128, 8.012510174242292393 ) ) ;
#3660 = DIRECTION ( 'NONE',  ( 1.000000000000000000, 0.000000000000000000, 0.000000000000000000 ) ) ;
#3661 = ITEM_DEFINED_TRANSFORMATION ( 'NONE', 'NONE', #4976,  #1587 ) ;
#3662 = EDGE_LOOP ( 'NONE', ( #7830, #1649, #7657, #827 ) ) ;
#3663 = ORIENTED_EDGE ( 'NONE', *, *, #7763, .T. ) ;
#3664 = ORIENTED_EDGE ( 'NONE', *, *, #1647, .T. ) ;
#3665 = ORIENTED_EDGE ( 'NONE', *, *, #4713, .T. ) ;
#3666 = EDGE_CURVE ( 'NONE', #6647, #7532, #1175, .T. ) ;
#3667 = LINE ( 'NONE', #494, #2252 ) ;
#3668 = LINE ( 'NONE', #2956, #2789 ) ;
#3669 = EDGE_CURVE ( 'NONE', #7873, #2445, #2366, .T. ) ;
#3670 = CARTESIAN_POINT ( 'NONE',  ( 0.000000000000000000, 0.000000000000000000, -2.700000000000001066 ) ) ;
#3671 = ORIENTED_EDGE ( 'NONE', *, *, #4538, .T. ) ;
#3672 = CARTESIAN_POINT ( 'NONE',  ( -3.469446951953613006E-15, 0.000000000000000000, 20.00000000000000355 ) ) ;
#3673 = VERTEX_POINT ( 'NONE', #4422 ) ;
#3674 = EDGE_CURVE ( 'NONE', #5083, #5864, #5560, .T. ) ;
#3675 = ORIENTED_EDGE ( 'NONE', *, *, #1370, .T. ) ;
#3676 = DIRECTION ( 'NONE',  ( 1.000000000000000000, 0.000000000000000000, 0.000000000000000000 ) ) ;
#3677 = CARTESIAN_POINT ( 'NONE',  ( -41.94165275491890554, 82.78620438794195024, -0.9356232805453277290 ) ) ;
#3678 = FACE_BOUND ( 'NONE', #3172, .T. ) ;
#3679 = ORIENTED_EDGE ( 'NONE', *, *, #3612, .T. ) ;
#3680 = ORIENTED_EDGE ( 'NONE', *, *, #3538, .T. ) ;
#3681 = CARTESIAN_POINT ( 'NONE',  ( 4.000000000000003553, -1.933795701539621659, -0.2488376576623028413 ) ) ;
#3682 = LINE ( 'NONE', #1778, #3561 ) ;
#3683 = CARTESIAN_POINT ( 'NONE',  ( 39.83716857408421674, 108.0000000000001421, 4.163336342344337027E-14 ) ) ;
#3684 = DIRECTION ( 'NONE',  ( 1.000000000000000000, 0.000000000000000000, 0.000000000000000000 ) ) ;
#3685 = AXIS2_PLACEMENT_3D ( 'NONE', #6420, #6958, #56 ) ;
#3686 = CARTESIAN_POINT ( 'NONE',  ( 2.000000000000000000, 1.773042676681340968, -2.276824562219559311E-15 ) ) ;
#3687 = AXIS2_PLACEMENT_3D ( 'NONE', #263, #7295, #5352 ) ;
#3688 = DIRECTION ( 'NONE',  ( 1.000000000000000000, 0.000000000000000000, 0.000000000000000000 ) ) ;
#3689 = ORIENTED_EDGE ( 'NONE', *, *, #8156, .T. ) ;
#3690 = AXIS2_PLACEMENT_3D ( 'NONE', #3339, #7845, #127 ) ;
#3691 = ORIENTED_EDGE ( 'NONE', *, *, #665, .T. ) ;
#3692 = DIRECTION ( 'NONE',  ( 0.000000000000000000, -1.000000000000000000, 1.026972870230479989E-15 ) ) ;
#3693 = EDGE_CURVE ( 'NONE', #7674, #2560, #5712, .T. ) ;
#3694 = CARTESIAN_POINT ( 'NONE',  ( 2.000000000000000000, -1.773042676681340524, 1.734723475976807094E-15 ) ) ;
#3695 = CARTESIAN_POINT ( 'NONE',  ( 4.200000000000001954, 0.000000000000000000, 0.000000000000000000 ) ) ;
#3696 = EDGE_CURVE ( 'NONE', #708, #2320, #5755, .T. ) ;
#3697 = DIRECTION ( 'NONE',  ( -1.000000000000000000, -0.000000000000000000, -0.000000000000000000 ) ) ;
#3698 = AXIS2_PLACEMENT_3D ( 'NONE', #1755, #2414, #6640 ) ;
#3699 = CARTESIAN_POINT ( 'NONE',  ( -1.198153218366585720E-14, 42.68016229225776925, 4.000000000000000000 ) ) ;
#3700 = CARTESIAN_POINT ( 'NONE',  ( 49.94236053903781425, 87.40012995604539014, -0.1563225272304197000 ) ) ;
#3701 = ORIENTED_EDGE ( 'NONE', *, *, #6498, .F. ) ;
#3702 = VECTOR ( 'NONE', #1847, 1000.000000000000000 ) ;
#3703 = CIRCLE ( 'NONE', #7468, 2.000000000000000888 ) ;
#3704 = AXIS2_PLACEMENT_3D ( 'NONE', #5303, #7164, #2212 ) ;
#3705 = VERTEX_POINT ( 'NONE', #2018 ) ;
#3706 = VECTOR ( 'NONE', #727, 1000.000000000000000 ) ;
#3707 = VECTOR ( 'NONE', #6102, 1000.000000000000000 ) ;
#3708 = B_SPLINE_CURVE_WITH_KNOTS ( 'NONE', 3,
 ( #175, #5381, #7893, #6659, #7937, #4672 ),
 .UNSPECIFIED., .F., .F.,
 ( 4, 2, 4 ),
 ( 0.002336974151641539512, 0.003500975885716449323, 0.004664977619791359567 ),
 .UNSPECIFIED. ) ;
#3709 = ORIENTED_EDGE ( 'NONE', *, *, #4735, .T. ) ;
#3710 = ORIENTED_EDGE ( 'NONE', *, *, #1521, .F. ) ;
#3711 = DIRECTION ( 'NONE',  ( 0.000000000000000000, -0.5000000000000011102, -0.8660254037844379305 ) ) ;
#3712 = DIRECTION ( 'NONE',  ( -1.000000000000000000, 0.000000000000000000, 0.000000000000000000 ) ) ;
#3713 = CARTESIAN_POINT ( 'NONE',  ( 4.999999999999993783, 6.123233995736758394E-16, 3.851859888774471706E-31 ) ) ;
#3714 = CIRCLE ( 'NONE', #2002, 39.00000000000002132 ) ;
#3715 = DIRECTION ( 'NONE',  ( 0.000000000000000000, 0.000000000000000000, 1.000000000000000000 ) ) ;
#3716 = CIRCLE ( 'NONE', #5834, 0.2000000000000000944 ) ;
#3717 = ORIENTED_EDGE ( 'NONE', *, *, #5660, .T. ) ;
#3718 = CARTESIAN_POINT ( 'NONE',  ( 49.99637462046962355, 84.37866470723844259, -2.323446361670104654 ) ) ;
#3719 = ADVANCED_FACE ( 'NONE', ( #1390, #3370 ), #3258, .F. ) ;
#3720 = ADVANCED_FACE ( 'NONE', ( #7224 ), #5824, .T. ) ;
#3721 = CIRCLE ( 'NONE', #3857, 2.649999999999995026 ) ;
#3722 = ORIENTED_EDGE ( 'NONE', *, *, #529, .F. ) ;
#3723 = EDGE_CURVE ( 'NONE', #4768, #7000, #1537, .T. ) ;
#3724 = ORIENTED_EDGE ( 'NONE', *, *, #5102, .F. ) ;
#3725 = AXIS2_PLACEMENT_3D ( 'NONE', #1039, #2870, #5412 ) ;
#3726 = VECTOR ( 'NONE', #2139, 1000.000000000000000 ) ;
#3727 = AXIS2_PLACEMENT_3D ( 'NONE', #1871, #8084, #3684 ) ;
#3728 = CARTESIAN_POINT ( 'NONE',  ( -29.99999999999999289, 30.00000000000000711, 10.00000000000000000 ) ) ;
#3729 = CARTESIAN_POINT ( 'NONE',  ( -41.99105870351831982, 84.12501143410540294, -2.238438502733109736 ) ) ;
#3730 = FACE_OUTER_BOUND ( 'NONE', #4854, .T. ) ;
#3731 = PRODUCT_DEFINITION_SHAPE ( 'NONE', 'NONE',  #8220 ) ;
#3732 = CIRCLE ( 'NONE', #3426, 4.000000000000000888 ) ;
#3733 = DIRECTION ( 'NONE',  ( -1.000000000000000000, 0.000000000000000000, 0.000000000000000000 ) ) ;
#3734 = CIRCLE ( 'NONE', #6243, 3.999999999999999112 ) ;
#3735 = PLANE ( 'NONE',  #2290 ) ;
#3736 = VERTEX_POINT ( 'NONE', #5866 ) ;
#3737 = ORIENTED_EDGE ( 'NONE', *, *, #5651, .F. ) ;
#3738 = PRESENTATION_STYLE_ASSIGNMENT (( #6167 ) ) ;
#3739 = CARTESIAN_POINT ( 'NONE',  ( 1.300000000000000044, 0.000000000000000000, 0.000000000000000000 ) ) ;
#3740 = DIRECTION ( 'NONE',  ( 0.000000000000000000, 0.000000000000000000, 1.000000000000000000 ) ) ;
#3741 = CARTESIAN_POINT ( 'NONE',  ( 9.020562060468115204E-14, -7.000000000000000000, 7.999999999999977796 ) ) ;
#3742 = CARTESIAN_POINT ( 'NONE',  ( -54.99999999999990052, 10.00000000000000000, 13.34999999999877573 ) ) ;
#3743 = DIRECTION ( 'NONE',  ( -1.000000000000000000, 0.000000000000000000, 0.000000000000000000 ) ) ;
#3744 = ADVANCED_FACE ( 'NONE', ( #3923 ), #788, .F. ) ;
#3745 = VERTEX_POINT ( 'NONE', #4615 ) ;
#3746 = DIRECTION ( 'NONE',  ( 1.000000000000000000, 0.000000000000000000, 0.000000000000000000 ) ) ;
#3747 = CARTESIAN_POINT ( 'NONE',  ( -3.000000000000000888, 45.09008114612887397, 0.000000000000000000 ) ) ;
#3748 = CYLINDRICAL_SURFACE ( 'NONE', #4895, 2.099999999999999645 ) ;
#3749 = CARTESIAN_POINT ( 'NONE',  ( 52.00000000000000000, -8.000000000000003553, 11.99999999999998934 ) ) ;
#3750 = EDGE_CURVE ( 'NONE', #4602, #1392, #825, .T. ) ;
#3751 = DIRECTION ( 'NONE',  ( 0.000000000000000000, 1.000000000000000000, 0.000000000000000000 ) ) ;
#3752 = CARTESIAN_POINT ( 'NONE',  ( 3.999999999999989786, -2.309401076758547777, -0.3572655899081733644 ) ) ;
#3753 = EDGE_LOOP ( 'NONE', ( #3591, #6487, #2609, #5360, #7242, #1797 ) ) ;
#3754 = ORIENTED_EDGE ( 'NONE', *, *, #718, .T. ) ;
#3755 = LINE ( 'NONE', #2047, #7283 ) ;
#3756 = PRODUCT_DEFINITION_CONTEXT ( 'detailed design', #5776, 'design' ) ;
#3757 = ORIENTED_EDGE ( 'NONE', *, *, #8049, .T. ) ;
#3758 = VECTOR ( 'NONE', #2159, 1000.000000000000000 ) ;
#3759 = ORIENTED_EDGE ( 'NONE', *, *, #2587, .T. ) ;
#3760 = CARTESIAN_POINT ( 'NONE',  ( -7.000000000000000000, 1.843750452292770530E-16, 8.033969604113661234 ) ) ;
#3761 = CARTESIAN_POINT ( 'NONE',  ( 52.00000000000000000, -8.000000000000003553, 19.99999999999998934 ) ) ;
#3762 = LINE ( 'NONE', #3132, #133 ) ;
#3763 = EDGE_CURVE ( 'NONE', #7604, #7241, #5790, .T. ) ;
#3764 = AXIS2_PLACEMENT_3D ( 'NONE', #3100, #6127, #6789 ) ;
#3765 = ORIENTED_EDGE ( 'NONE', *, *, #7645, .T. ) ;
#3766 = ADVANCED_FACE ( 'NONE', ( #3407 ), #164, .F. ) ;
#3767 = CARTESIAN_POINT ( 'NONE',  ( 39.83716857408421674, 108.0000000000001990, -4.999999999999976907 ) ) ;
#3768 = ORIENTED_EDGE ( 'NONE', *, *, #6153, .F. ) ;
#3769 = ORIENTED_EDGE ( 'NONE', *, *, #4238, .F. ) ;
#3770 = DIRECTION ( 'NONE',  ( 0.000000000000000000, 0.000000000000000000, 1.000000000000000000 ) ) ;
#3771 = EDGE_CURVE ( 'NONE', #5524, #855, #4007, .T. ) ;
#3772 = CARTESIAN_POINT ( 'NONE',  ( -41.95747712235106519, 83.10910067217422181, -1.483502059617906266 ) ) ;
#3773 = CARTESIAN_POINT ( 'NONE',  ( -29.99999999999999289, 30.00000000000000711, 10.00000000000000000 ) ) ;
#3774 = CIRCLE ( 'NONE', #4773, 1.535500000000000087 ) ;
#3775 = DIRECTION ( 'NONE',  ( -1.000000000000000000, 0.000000000000000000, 0.000000000000000000 ) ) ;
#3776 = CARTESIAN_POINT ( 'NONE',  ( 2.000000000000000000, 1.773042676681340968, -2.276824562219559311E-15 ) ) ;
#3777 = PRESENTATION_LAYER_ASSIGNMENT (  '', '', ( #1106 ) ) ;
#3778 = VERTEX_POINT ( 'NONE', #236 ) ;
#3779 = ORIENTED_EDGE ( 'NONE', *, *, #7159, .T. ) ;
#3780 = DIRECTION ( 'NONE',  ( 0.000000000000000000, 0.000000000000000000, -1.000000000000000000 ) ) ;
#3781 = DIRECTION ( 'NONE',  ( -1.000000000000000000, -0.000000000000000000, -0.000000000000000000 ) ) ;
#3782 = CARTESIAN_POINT ( 'NONE',  ( 2.000000000000000000, 1.773042676681340968, -2.276824562219559311E-15 ) ) ;
#3783 = LINE ( 'NONE', #4402, #7162 ) ;
#3784 =( GEOMETRIC_REPRESENTATION_CONTEXT ( 3 ) GLOBAL_UNCERTAINTY_ASSIGNED_CONTEXT ( ( #819 ) ) GLOBAL_UNIT_ASSIGNED_CONTEXT ( ( #4668, #2873, #6608 ) ) REPRESENTATION_CONTEXT ( 'NONE', 'WORKASPACE' ) );
#3785 = CARTESIAN_POINT ( 'NONE',  ( 1.300000000000000044, 0.000000000000000000, 0.000000000000000000 ) ) ;
#3786 = DIRECTION ( 'NONE',  ( 0.000000000000000000, 0.000000000000000000, 1.000000000000000000 ) ) ;
#3787 = EDGE_CURVE ( 'NONE', #2420, #5760, #3555, .T. ) ;
#3788 = ORIENTED_EDGE ( 'NONE', *, *, #3613, .T. ) ;
#3789 = LINE ( 'NONE', #6972, #4580 ) ;
#3790 = DIRECTION ( 'NONE',  ( -0.000000000000000000, -0.000000000000000000, 1.000000000000000000 ) ) ;
#3791 = DIRECTION ( 'NONE',  ( 0.000000000000000000, -1.000000000000000000, 0.000000000000000000 ) ) ;
#3792 = CARTESIAN_POINT ( 'NONE',  ( -3.000000000000000888, 45.09008114612887397, 4.000000000000000000 ) ) ;
#3793 = CARTESIAN_POINT ( 'NONE',  ( 49.98627395458714062, 86.20659363562862154, 2.098057260256863010 ) ) ;
#3794 = ORIENTED_EDGE ( 'NONE', *, *, #5726, .F. ) ;
#3795 = ORIENTED_EDGE ( 'NONE', *, *, #2706, .T. ) ;
#3796 = LINE ( 'NONE', #3285, #6231 ) ;
#3797 = ORIENTED_EDGE ( 'NONE', *, *, #7727, .T. ) ;
#3798 = EDGE_LOOP ( 'NONE', ( #1344, #564, #1775 ) ) ;
#3799 = PRODUCT_DEFINITION_SHAPE ( 'NONE', 'NONE',  #8206 ) ;
#3800 = CYLINDRICAL_SURFACE ( 'NONE', #6357, 2.500000000000002220 ) ;
#3801 = DIRECTION ( 'NONE',  ( -0.000000000000000000, -0.000000000000000000, 1.000000000000000000 ) ) ;
#3802 = DIRECTION ( 'NONE',  ( -1.000000000000000000, -0.000000000000000000, -0.000000000000000000 ) ) ;
#3803 = DIRECTION ( 'NONE',  ( -5.692221470121481927E-17, 1.000000000000000000, 1.363075293218192124E-18 ) ) ;
#3804 = ORIENTED_EDGE ( 'NONE', *, *, #5188, .F. ) ;
#3805 = CARTESIAN_POINT ( 'NONE',  ( -39.83716857408418122, 108.0000000000001421, 4.163336342344337027E-14 ) ) ;
#3806 = ORIENTED_EDGE ( 'NONE', *, *, #1369, .T. ) ;
#3807 = ORIENTED_EDGE ( 'NONE', *, *, #8141, .T. ) ;
#3808 = EDGE_CURVE ( 'NONE', #4068, #4539, #6593, .T. ) ;
#3809 = EDGE_CURVE ( 'NONE', #4663, #7226, #362, .T. ) ;
#3810 = B_SPLINE_CURVE_WITH_KNOTS ( 'NONE', 3,
 ( #701, #7608, #1338, #4994, #3247, #7514 ),
 .UNSPECIFIED., .F., .F.,
 ( 4, 2, 4 ),
 ( 0.002336974151641540379, 0.003500975885716449323, 0.004664977619791357832 ),
 .UNSPECIFIED. ) ;
#3811 = LINE ( 'NONE', #1225, #2247 ) ;
#3812 = ADVANCED_FACE ( 'NONE', ( #7803 ), #1561, .F. ) ;
#3813 = CARTESIAN_POINT ( 'NONE',  ( 41.99757081983620566, 85.51235667645809713, -2.358461006662995629 ) ) ;
#3814 = CARTESIAN_POINT ( 'NONE',  ( 2.000000000000000000, -1.877893248421449134E-15, -1.535500000000000087 ) ) ;
#3815 = SURFACE_SIDE_STYLE ('',( #4627 ) ) ;
#3816 = AXIS2_PLACEMENT_3D ( 'NONE', #1852, #4382, #2511 ) ;
#3817 = CARTESIAN_POINT ( 'NONE',  ( 0.000000000000000000, 0.000000000000000000, -2.700000000000001066 ) ) ;
#3818 = APPLICATION_CONTEXT ( 'automotive_design' ) ;
#3819 = ORIENTED_EDGE ( 'NONE', *, *, #2167, .F. ) ;
#3820 = VECTOR ( 'NONE', #7056, 1000.000000000000000 ) ;
#3821 = AXIS2_PLACEMENT_3D ( 'NONE', #8088, #8165, #3786 ) ;
#3822 =( NAMED_UNIT ( * ) PLANE_ANGLE_UNIT ( ) SI_UNIT ( $, .RADIAN. ) );
#3823 = DIRECTION ( 'NONE',  ( -1.000000000000000000, 0.000000000000000000, 0.000000000000000000 ) ) ;
#3824 = FACE_OUTER_BOUND ( 'NONE', #7646, .T. ) ;
#3825 = CARTESIAN_POINT ( 'NONE',  ( -39.83716857408418122, 108.0000000000001990, -4.999999999999976907 ) ) ;
#3826 = DIRECTION ( 'NONE',  ( 0.000000000000000000, 0.000000000000000000, -1.000000000000000000 ) ) ;
#3827 = CARTESIAN_POINT ( 'NONE',  ( -31.74999999999995737, 0.000000000000000000, 0.000000000000000000 ) ) ;
#3828 = ORIENTED_EDGE ( 'NONE', *, *, #6168, .T. ) ;
#3829 = CARTESIAN_POINT ( 'NONE',  ( 35.00000000000000000, -29.99999999999997868, 10.00000000000000000 ) ) ;
#3830 = DIRECTION ( 'NONE',  ( 0.000000000000000000, -0.5000000000000011102, -0.8660254037844379305 ) ) ;
#3831 = CARTESIAN_POINT ( 'NONE',  ( 2.999999999999999112, 45.09008114612887397, 4.000000000000000000 ) ) ;
#3832 = CIRCLE ( 'NONE', #1436, 1.599999999999986766 ) ;
#3833 = LINE ( 'NONE', #2453, #104 ) ;
#3834 = DIRECTION ( 'NONE',  ( 0.000000000000000000, -0.5000000000000011102, -0.8660254037844379305 ) ) ;
#3835 = ORIENTED_EDGE ( 'NONE', *, *, #3808, .T. ) ;
#3836 = EDGE_CURVE ( 'NONE', #8077, #4814, #4658, .T. ) ;
#3837 = AXIS2_PLACEMENT_3D ( 'NONE', #3435, #2310, #2223 ) ;
#3838 = VERTEX_POINT ( 'NONE', #3290 ) ;
#3839 = CARTESIAN_POINT ( 'NONE',  ( 2.000000000000000000, -1.773042676681340968, 2.059984127722458425E-15 ) ) ;
#3840 = AXIS2_PLACEMENT_3D ( 'NONE', #5812, #5274, #5241 ) ;
#3841 = ORIENTED_EDGE ( 'NONE', *, *, #7096, .F. ) ;
#3842 = ORIENTED_EDGE ( 'NONE', *, *, #2805, .F. ) ;
#3843 = DIRECTION ( 'NONE',  ( 0.8571673007021125557, 2.194743421410585277E-16, -0.5150380749100536004 ) ) ;
#3844 = DIRECTION ( 'NONE',  ( 1.000000000000000000, 0.000000000000000000, 0.000000000000000000 ) ) ;
#3845 = DIRECTION ( 'NONE',  ( 1.412205397084881070E-17, -2.775557561562891967E-17, -1.000000000000000000 ) ) ;
#3846 = CLOSED_SHELL ( 'NONE', ( #2105, #1442, #6536, #6569, #4049, #1823, #6764, #3766, #464, #1468, #7636, #1948, #2829, #4673, #3272, #1386, #3034, #3387, #4265, #7160, #7121, #5937, #810, #8071, #1592, #922, #964, #5339 ) ) ;
#3847 = AXIS2_PLACEMENT_3D ( 'NONE', #484, #2489, #5034 ) ;
#3848 = ORIENTED_EDGE ( 'NONE', *, *, #1630, .T. ) ;
#3849 = EDGE_LOOP ( 'NONE', ( #2194, #3046, #7524, #6022 ) ) ;
#3850 = ADVANCED_FACE ( 'NONE', ( #1502 ), #5331, .F. ) ;
#3851 = VERTEX_POINT ( 'NONE', #4697 ) ;
#3852 =( GEOMETRIC_REPRESENTATION_CONTEXT ( 3 ) GLOBAL_UNCERTAINTY_ASSIGNED_CONTEXT ( ( #169 ) ) GLOBAL_UNIT_ASSIGNED_CONTEXT ( ( #2071, #1450, #3991 ) ) REPRESENTATION_CONTEXT ( 'NONE', 'WORKASPACE' ) );
#3853 = VECTOR ( 'NONE', #7746, 1000.000000000000000 ) ;
#3854 = CARTESIAN_POINT ( 'NONE',  ( 1.300000000000000044, 0.000000000000000000, 0.000000000000000000 ) ) ;
#3855 = DIRECTION ( 'NONE',  ( -1.000000000000000000, -0.000000000000000000, -0.000000000000000000 ) ) ;
#3856 = CARTESIAN_POINT ( 'NONE',  ( -29.99999999999999289, 30.00000000000000711, 1.734723475976807094E-15 ) ) ;
#3857 = AXIS2_PLACEMENT_3D ( 'NONE', #3015, #7554, #4227 ) ;
#3858 = DIRECTION ( 'NONE',  ( 0.000000000000000000, 0.000000000000000000, 1.000000000000000000 ) ) ;
#3859 = VECTOR ( 'NONE', #6199, 1000.000000000000000 ) ;
#3860 = EDGE_CURVE ( 'NONE', #4570, #3458, #7734, .T. ) ;
#3861 = VECTOR ( 'NONE', #1404, 1000.000000000000000 ) ;
#3862 = PRESENTATION_LAYER_ASSIGNMENT (  '', '', ( #7288 ) ) ;
#3863 = EDGE_LOOP ( 'NONE', ( #6824, #1341, #5143, #7767 ) ) ;
#3864 = LINE ( 'NONE', #7668, #3429 ) ;
#3865 = CARTESIAN_POINT ( 'NONE',  ( 5.200000000000020606, 3.306546357697854226E-16, 2.699999999999993516 ) ) ;
#3866 = DIRECTION ( 'NONE',  ( -1.000000000000000000, 0.000000000000000000, 0.000000000000000000 ) ) ;
#3867 = VECTOR ( 'NONE', #79, 1000.000000000000114 ) ;
#3868 = DIRECTION ( 'NONE',  ( -1.000000000000000000, 0.000000000000000000, -0.000000000000000000 ) ) ;
#3869 = CARTESIAN_POINT ( 'NONE',  ( -50.00000000000000711, 85.15661249647207853, -2.400000000000023448 ) ) ;
#3870 = EDGE_LOOP ( 'NONE', ( #7901, #5941, #584, #5279 ) ) ;
#3871 = CARTESIAN_POINT ( 'NONE',  ( 4.000000000000003553, 0.000000000000000000, 0.000000000000000000 ) ) ;
#3872 = PRESENTATION_STYLE_ASSIGNMENT (( #6460 ) ) ;
#3873 = DIRECTION ( 'NONE',  ( -1.000000000000000000, 0.000000000000000000, 0.000000000000000000 ) ) ;
#3874 = CARTESIAN_POINT ( 'NONE',  ( 2.000000000000000000, -0.8865213383406690406, 1.535500000000000975 ) ) ;
#3875 = EDGE_CURVE ( 'NONE', #5793, #7610, #2199, .T. ) ;
#3876 = ORIENTED_EDGE ( 'NONE', *, *, #6630, .T. ) ;
#3877 = EDGE_CURVE ( 'NONE', #2510, #6584, #1030, .T. ) ;
#3878 = ORIENTED_EDGE ( 'NONE', *, *, #6916, .F. ) ;
#3879 = LINE ( 'NONE', #8177, #6752 ) ;
#3880 = ORIENTED_EDGE ( 'NONE', *, *, #3696, .F. ) ;
#3881 = VERTEX_POINT ( 'NONE', #6059 ) ;
#3882 = DIRECTION ( 'NONE',  ( -0.000000000000000000, -0.000000000000000000, 1.000000000000000000 ) ) ;
#3883 = DIRECTION ( 'NONE',  ( 0.000000000000000000, 0.000000000000000000, 1.000000000000000000 ) ) ;
#3884 = CARTESIAN_POINT ( 'NONE',  ( 2.000000000000010658, -3.464101615137748169, 0.000000000000000000 ) ) ;
#3885 = DIRECTION ( 'NONE',  ( -1.000000000000000000, 3.622251695638288984E-16, 3.469446951953613418E-18 ) ) ;
#3886 = EDGE_LOOP ( 'NONE', ( #7585, #1911, #5612, #8186 ) ) ;
#3887 = AXIS2_PLACEMENT_3D ( 'NONE', #1832, #4359, #4907 ) ;
#3888 = ORIENTED_EDGE ( 'NONE', *, *, #1826, .T. ) ;
#3889 = ORIENTED_EDGE ( 'NONE', *, *, #7737, .F. ) ;
#3890 = ADVANCED_FACE ( 'NONE', ( #1078 ), #1583, .T. ) ;
#3891 = B_SPLINE_CURVE_WITH_KNOTS ( 'NONE', 3,
 ( #7729, #6367, #7690, #2552, #3252, #1296, #6942, #1888 ),
 .UNSPECIFIED., .F., .F.,
 ( 4, 2, 2, 4 ),
 ( 0.007505023096728393080, 0.007854877166616045306, 0.008204731236503698399, 0.008904439376279002852 ),
 .UNSPECIFIED. ) ;
#3892 = FACE_OUTER_BOUND ( 'NONE', #5752, .T. ) ;
#3893 = FACE_OUTER_BOUND ( 'NONE', #5465, .T. ) ;
#3894 = DIRECTION ( 'NONE',  ( 0.000000000000000000, -1.000000000000000000, 1.026972870230479989E-15 ) ) ;
#3895 = ADVANCED_FACE ( 'NONE', ( #4782 ), #4909, .F. ) ;
#3896 = AXIS2_PLACEMENT_3D ( 'NONE', #7541, #561, #5641 ) ;
#3897 = EDGE_CURVE ( 'NONE', #1038, #3653, #6641, .T. ) ;
#3898 = DIRECTION ( 'NONE',  ( 1.000000000000000000, 1.502586498047605218E-16, -1.412205397084881070E-17 ) ) ;
#3899 = DIRECTION ( 'NONE',  ( -1.000000000000000000, -0.000000000000000000, -0.000000000000000000 ) ) ;
#3900 = CARTESIAN_POINT ( 'NONE',  ( 52.00000000000000000, -8.000000000000003553, 11.99999999999998934 ) ) ;
#3901 = DIRECTION ( 'NONE',  ( 1.412205397084881070E-17, -2.775557561562891967E-17, -1.000000000000000000 ) ) ;
#3902 = CARTESIAN_POINT ( 'NONE',  ( 55.00000000000000000, 10.00000000000000000, 15.50000000000000355 ) ) ;
#3903 = COLOUR_RGB ( '', 0.40784314, 0.44705882, 0.49803922) ;
#3904 = CARTESIAN_POINT ( 'NONE',  ( -49.97874610126634565, 86.47445480916303495, -1.919346332466802085 ) ) ;
#3905 = ORIENTED_EDGE ( 'NONE', *, *, #6208, .T. ) ;
#3906 = LINE ( 'NONE', #696, #5773 ) ;
#3907 = EDGE_CURVE ( 'NONE', #6596, #4602, #4732, .T. ) ;
#3908 = CARTESIAN_POINT ( 'NONE',  ( 2.000000000000000000, 1.773042676681340968, -2.276824562219559311E-15 ) ) ;
#3909 = DIRECTION ( 'NONE',  ( -0.000000000000000000, -0.000000000000000000, 1.000000000000000000 ) ) ;
#3910 = DIRECTION ( 'NONE',  ( 0.000000000000000000, -0.4999999999999990563, 0.8660254037844391517 ) ) ;
#3911 = EDGE_CURVE ( 'NONE', #6759, #2831, #1441, .T. ) ;
#3912 = DIRECTION ( 'NONE',  ( -0.000000000000000000, 0.8660254037844391517, 0.4999999999999990563 ) ) ;
#3913 = VERTEX_POINT ( 'NONE', #361 ) ;
#3914 = AXIS2_PLACEMENT_3D ( 'NONE', #6376, #2631, #5100 ) ;
#3915 = ORIENTED_EDGE ( 'NONE', *, *, #2736, .F. ) ;
#3916 = SHAPE_REPRESENTATION ( 'BR-153', ( #3115, #2967, #7623, #442, #3914, #5118, #1513, #7210, #5770, #3638, #1111, #305, #4976, #298, #4971, #3502, #4567, #976 ), #3505 ) ;
#3917 = CARTESIAN_POINT ( 'NONE',  ( -4.000000000000000000, 0.000000000000000000, -2.700000000000000178 ) ) ;
#3918 = VERTEX_POINT ( 'NONE', #6683 ) ;
#3919 = ORIENTED_EDGE ( 'NONE', *, *, #754, .T. ) ;
#3920 = DIRECTION ( 'NONE',  ( 0.000000000000000000, 0.000000000000000000, -1.000000000000000000 ) ) ;
#3921 = AXIS2_PLACEMENT_3D ( 'NONE', #1448, #262, #5853 ) ;
#3922 = CARTESIAN_POINT ( 'NONE',  ( -4.000000000000000000, 2.309401076758496263, -2.700000000000000178 ) ) ;
#3923 = FACE_OUTER_BOUND ( 'NONE', #6027, .T. ) ;
#3924 = DIRECTION ( 'NONE',  ( -0.7858905944355958351, -0.6183655662936492492, -4.916232611899799311E-17 ) ) ;
#3925 =( REPRESENTATION_RELATIONSHIP ('NONE','NONE', #3916, #7239 ) REPRESENTATION_RELATIONSHIP_WITH_TRANSFORMATION ( #2162 )SHAPE_REPRESENTATION_RELATIONSHIP( ) );
#3926 = ORIENTED_EDGE ( 'NONE', *, *, #5689, .F. ) ;
#3927 = ADVANCED_FACE ( 'NONE', ( #7262 ), #6592, .T. ) ;
#3928 = ORIENTED_EDGE ( 'NONE', *, *, #2057, .T. ) ;
#3929 = EDGE_LOOP ( 'NONE', ( #8122, #2729, #5371, #7502 ) ) ;
#3930 = EDGE_CURVE ( 'NONE', #5524, #4602, #5551, .T. ) ;
#3931 = CARTESIAN_POINT ( 'NONE',  ( 1.300000000000000044, 0.000000000000000000, 0.000000000000000000 ) ) ;
#3932 = CARTESIAN_POINT ( 'NONE',  ( 41.94721337724063659, 82.88985491569346209, -1.171319538143684280 ) ) ;
#3933 = CARTESIAN_POINT ( 'NONE',  ( -54.99999999999990052, -10.00000000000000000, 15.49999999999877254 ) ) ;
#3934 = MANIFOLD_SOLID_BREP ( 'Hex', #7012 ) ;
#3935 = VERTEX_POINT ( 'NONE', #7387 ) ;
#3936 = FILL_AREA_STYLE ('',( #7628 ) ) ;
#3937 = EDGE_CURVE ( 'NONE', #3962, #1975, #1706, .T. ) ;
#3938 = EDGE_CURVE ( 'NONE', #2320, #3388, #3621, .T. ) ;
#3939 = CARTESIAN_POINT ( 'NONE',  ( -27.34999999999999076, 30.00000000000000711, 4.599999999999997868 ) ) ;
#3940 = CARTESIAN_POINT ( 'NONE',  ( 0.1499999999999973577, 3.184081677783118191E-16, -2.600000000000000089 ) ) ;
#3941 = MECHANICAL_DESIGN_GEOMETRIC_PRESENTATION_REPRESENTATION (  '', ( #8099 ), #3143 ) ;
#3942 = CARTESIAN_POINT ( 'NONE',  ( 0.000000000000000000, 0.000000000000000000, 0.000000000000000000 ) ) ;
#3943 = DIRECTION ( 'NONE',  ( 0.000000000000000000, 0.000000000000000000, -1.000000000000000000 ) ) ;
#3944 = CARTESIAN_POINT ( 'NONE',  ( -49.97491191256673915, 86.58758952877983006, 1.806678789609362124 ) ) ;
#3945 = VECTOR ( 'NONE', #1000, 1000.000000000000000 ) ;
#3946 = VERTEX_POINT ( 'NONE', #449 ) ;
#3947 = CARTESIAN_POINT ( 'NONE',  ( -39.83716857408418122, 108.0000000000001137, 0.7510757737844986348 ) ) ;
#3948 = FILL_AREA_STYLE_COLOUR ( '', #4617 ) ;
#3949 = LINE ( 'NONE', #7786, #7118 ) ;
#3950 = DIRECTION ( 'NONE',  ( -1.000000000000000000, -0.000000000000000000, -0.000000000000000000 ) ) ;
#3951 = FACE_OUTER_BOUND ( 'NONE', #671, .T. ) ;
#3952 = VERTEX_POINT ( 'NONE', #8045 ) ;
#3953 = FACE_OUTER_BOUND ( 'NONE', #7188, .T. ) ;
#3954 = VERTEX_POINT ( 'NONE', #2363 ) ;
#3955 = ORIENTED_EDGE ( 'NONE', *, *, #3647, .T. ) ;
#3956 = ORIENTED_EDGE ( 'NONE', *, *, #7943, .T. ) ;
#3957 = ORIENTED_EDGE ( 'NONE', *, *, #7710, .F. ) ;
#3958 = CARTESIAN_POINT ( 'NONE',  ( 2.000000000000000000, 1.773042676681340968, -2.276824562219559311E-15 ) ) ;
#3959 = CARTESIAN_POINT ( 'NONE',  ( 50.00000000000000000, 9.332579536216795825E-15, 54.99999999999997868 ) ) ;
#3960 = DIRECTION ( 'NONE',  ( 6.123233995736766036E-17, -1.000000000000000000, -1.363075293218192124E-18 ) ) ;
#3961 = AXIS2_PLACEMENT_3D ( 'NONE', #3773, #7626, #598 ) ;
#3962 = VERTEX_POINT ( 'NONE', #616 ) ;
#3963 = ORIENTED_EDGE ( 'NONE', *, *, #4149, .T. ) ;
#3964 = ORIENTED_EDGE ( 'NONE', *, *, #687, .F. ) ;
#3965 = VECTOR ( 'NONE', #2585, 1000.000000000000000 ) ;
#3966 = CARTESIAN_POINT ( 'NONE',  ( -41.08716857408418122, 108.0000000000001421, 4.161571085597980959E-14 ) ) ;
#3967 = CARTESIAN_POINT ( 'NONE',  ( 41.95061225082201162, 87.03752755116852313, -1.274660781186774283 ) ) ;
#3968 = LINE ( 'NONE', #5908, #880 ) ;
#3969 = TOROIDAL_SURFACE ( 'NONE', #5419, 3.299999999999999822, 0.2000000000000000111 ) ;
#3970 = AXIS2_PLACEMENT_3D ( 'NONE', #5452, #989, #6058 ) ;
#3971 = FILL_AREA_STYLE_COLOUR ( '', #7994 ) ;
#3972 = EDGE_CURVE ( 'NONE', #3364, #3553, #3246, .T. ) ;
#3973 = EDGE_CURVE ( 'NONE', #7290, #7075, #5025, .T. ) ;
#3974 = EDGE_CURVE ( 'NONE', #1812, #3296, #1154, .T. ) ;
#3975 = AXIS2_PLACEMENT_3D ( 'NONE', #2086, #7144, #6554 ) ;
#3976 = VECTOR ( 'NONE', #8095, 1000.000000000000114 ) ;
#3977 = AXIS2_PLACEMENT_3D ( 'NONE', #1771, #1091, #5636 ) ;
#3978 = CONICAL_SURFACE ( 'NONE', #654, 1.250000000000001110, 1.029744258676655200 ) ;
#3979 = B_SPLINE_CURVE_WITH_KNOTS ( 'NONE', 3,
 ( #2302, #423, #4837, #6867, #3597, #2964 ),
 .UNSPECIFIED., .F., .F.,
 ( 4, 2, 4 ),
 ( 0.006106730743980896305, 0.006805876920354644692, 0.007505023096728393080 ),
 .UNSPECIFIED. ) ;
#3980 = CARTESIAN_POINT ( 'NONE',  ( 0.1499999999999973577, 3.367778697655221012E-16, -2.750000000000000000 ) ) ;
#3981 = CARTESIAN_POINT ( 'NONE',  ( 42.00000000000003553, 85.00000000000012790, -2.399999999999999023 ) ) ;
#3982 = CARTESIAN_POINT ( 'NONE',  ( 2.500000000000002220, 2.357898499370434386, -3.469446951953614189E-15 ) ) ;
#3983 = CIRCLE ( 'NONE', #6888, 3.500000000000000000 ) ;
#3984 = DIRECTION ( 'NONE',  ( 0.000000000000000000, 0.000000000000000000, 1.000000000000000000 ) ) ;
#3985 = AXIS2_PLACEMENT_3D ( 'NONE', #7983, #5913, #4674 ) ;
#3986 = CARTESIAN_POINT ( 'NONE',  ( -49.95669389512426761, 87.08239168930829521, -1.203442334140364389 ) ) ;
#3987 = EDGE_LOOP ( 'NONE', ( #5458, #440, #7501, #3584, #1559, #5252 ) ) ;
#3988 = LINE ( 'NONE', #2107, #3375 ) ;
#3989 = AXIS2_PLACEMENT_3D ( 'NONE', #4014, #5907, #996 ) ;
#3990 = AXIS2_PLACEMENT_3D ( 'NONE', #6435, #2113, #5857 ) ;
#3991 =( NAMED_UNIT ( * ) SI_UNIT ( $, .STERADIAN. ) SOLID_ANGLE_UNIT ( ) );
#3992 = CARTESIAN_POINT ( 'NONE',  ( -54.99999999999990052, -10.00000000000000000, 17.64999999999876223 ) ) ;
#3993 = CARTESIAN_POINT ( 'NONE',  ( 0.6543461111163468846, 4.241015250120812929, -0.1391502195351439208 ) ) ;
#3994 = LINE ( 'NONE', #4489, #5448 ) ;
#3995 = EDGE_CURVE ( 'NONE', #1678, #7038, #2415, .T. ) ;
#3996 = ORIENTED_EDGE ( 'NONE', *, *, #7737, .T. ) ;
#3997 = AXIS2_PLACEMENT_3D ( 'NONE', #3817, #6336, #5380 ) ;
#3998 = CARTESIAN_POINT ( 'NONE',  ( 50.00000000000008527, 84.84140190613213406, -2.399999999999993250 ) ) ;
#3999 = UNCERTAINTY_MEASURE_WITH_UNIT (LENGTH_MEASURE( 1.000000000000000082E-05 ), #7707, 'distance_accuracy_value', 'NONE');
#4000 = AXIS2_PLACEMENT_3D ( 'NONE', #2650, #7779, #2065 ) ;
#4001 = ORIENTED_EDGE ( 'NONE', *, *, #4356, .T. ) ;
#4002 = EDGE_LOOP ( 'NONE', ( #4134, #7109, #3512, #864 ) ) ;
#4003 = TOROIDAL_SURFACE ( 'NONE', #1477, 2.600000000000000089, 0.1499999999999999944 ) ;
#4004 = ADVANCED_FACE ( 'NONE', ( #5128 ), #7480, .F. ) ;
#4005 = CARTESIAN_POINT ( 'NONE',  ( 7.000000000000000000, 8.572527594031473190E-16, 8.000000000000000000 ) ) ;
#4006 = PLANE ( 'NONE',  #3032 ) ;
#4007 = LINE ( 'NONE', #4546, #7264 ) ;
#4008 = APPLICATION_PROTOCOL_DEFINITION ( 'draft international standard', 'automotive_design', 1998, #4223 ) ;
#4009 = EDGE_LOOP ( 'NONE', ( #1520, #1757, #3503 ) ) ;
#4010 = ORIENTED_EDGE ( 'NONE', *, *, #5389, .F. ) ;
#4011 = ORIENTED_EDGE ( 'NONE', *, *, #2095, .T. ) ;
#4012 = DIRECTION ( 'NONE',  ( 0.000000000000000000, -1.000000000000000000, 1.287488025362403787E-15 ) ) ;
#4013 = EDGE_CURVE ( 'NONE', #7532, #2900, #1209, .T. ) ;
#4014 = CARTESIAN_POINT ( 'NONE',  ( 60.00000000000000711, 9.332579536216795825E-15, 54.99999999999997868 ) ) ;
#4015 = CARTESIAN_POINT ( 'NONE',  ( 2.000000000000027089, 3.464101615137739731, 0.000000000000000000 ) ) ;
#4016 = ADVANCED_FACE ( 'NONE', ( #4283 ), #5620, .T. ) ;
#4017 = DIRECTION ( 'NONE',  ( 0.000000000000000000, 0.000000000000000000, -1.000000000000000000 ) ) ;
#4018 = EDGE_CURVE ( 'NONE', #3366, #452, #6977, .T. ) ;
#4019 = DIRECTION ( 'NONE',  ( -1.000000000000000000, -0.000000000000000000, -0.000000000000000000 ) ) ;
#4020 = CARTESIAN_POINT ( 'NONE',  ( 5.930697612239895941E-15, 38.99999999999999289, -4.999999999999990230 ) ) ;
#4021 = DIRECTION ( 'NONE',  ( -0.000000000000000000, 1.000000000000000000, -0.000000000000000000 ) ) ;
#4022 = CARTESIAN_POINT ( 'NONE',  ( 0.000000000000000000, 0.000000000000000000, 5.400000000000002132 ) ) ;
#4023 = CARTESIAN_POINT ( 'NONE',  ( 2.000000000000027089, 3.464101615137739731, -2.700000000000001066 ) ) ;
#4024 = EDGE_CURVE ( 'NONE', #6597, #2793, #1118, .T. ) ;
#4025 = ORIENTED_EDGE ( 'NONE', *, *, #2391, .F. ) ;
#4026 = CARTESIAN_POINT ( 'NONE',  ( 2.000000000000000000, 1.329782007511004727, -0.7677500000000019309 ) ) ;
#4027 = EDGE_CURVE ( 'NONE', #1969, #992, #3027, .T. ) ;
#4028 = CARTESIAN_POINT ( 'NONE',  ( 2.500000000000002220, 1.178949249685218970, 2.041999999999998483 ) ) ;
#4029 = DIRECTION ( 'NONE',  ( -1.000000000000000000, -0.000000000000000000, -0.000000000000000000 ) ) ;
#4030 = CARTESIAN_POINT ( 'NONE',  ( -49.97875682971460520, 83.53682071867368109, 1.908850074583584355 ) ) ;
#4031 = LINE ( 'NONE', #6007, #6520 ) ;
#4032 = VERTEX_POINT ( 'NONE', #2454 ) ;
#4033 = DIRECTION ( 'NONE',  ( -0.000000000000000000, 1.000000000000000000, -0.000000000000000000 ) ) ;
#4034 = EDGE_CURVE ( 'NONE', #2847, #7631, #7132, .T. ) ;
#4035 = ORIENTED_EDGE ( 'NONE', *, *, #2354, .T. ) ;
#4036 = EDGE_LOOP ( 'NONE', ( #3691, #1413, #854 ) ) ;
#4037 = LINE ( 'NONE', #4005, #4894 ) ;
#4038 = DIRECTION ( 'NONE',  ( 0.000000000000000000, -0.5000000000000011102, -0.8660254037844379305 ) ) ;
#4039 = DIRECTION ( 'NONE',  ( -0.000000000000000000, -0.000000000000000000, 1.000000000000000000 ) ) ;
#4040 = ORIENTED_EDGE ( 'NONE', *, *, #4829, .T. ) ;
#4041 = ORIENTED_EDGE ( 'NONE', *, *, #7515, .F. ) ;
#4042 = EDGE_LOOP ( 'NONE', ( #5816, #1190, #4788 ) ) ;
#4043 = VECTOR ( 'NONE', #6933, 1000.000000000000000 ) ;
#4044 = CARTESIAN_POINT ( 'NONE',  ( 0.000000000000000000, 0.000000000000000000, -2.674599999999998978 ) ) ;
#4045 = CARTESIAN_POINT ( 'NONE',  ( -41.99057649487198063, 85.91769722991278968, 2.230045660306874566 ) ) ;
#4046 = CARTESIAN_POINT ( 'NONE',  ( -2.650000000000010125, 0.000000000000000000, 5.400000000000002132 ) ) ;
#4047 = DIRECTION ( 'NONE',  ( -1.000000000000000000, 0.000000000000000000, 1.412205397084726379E-17 ) ) ;
#4048 = EDGE_CURVE ( 'NONE', #6979, #1855, #4744, .T. ) ;
#4049 = ADVANCED_FACE ( 'NONE', ( #5780 ), #2726, .F. ) ;
#4050 = EDGE_CURVE ( 'NONE', #5018, #741, #3994, .T. ) ;
#4051 = CARTESIAN_POINT ( 'NONE',  ( 2.099999999999999645, 0.000000000000000000, -2.394516984716111185 ) ) ;
#4052 = CARTESIAN_POINT ( 'NONE',  ( 58.00000000000000000, -8.000000000000000000, -8.000000000000000000 ) ) ;
#4053 = DIRECTION ( 'NONE',  ( -0.000000000000000000, -0.000000000000000000, -1.000000000000000000 ) ) ;
#4054 = CARTESIAN_POINT ( 'NONE',  ( 6.631756180578551430, 2.252199472339280195, 8.030486436084467883 ) ) ;
#4055 = EDGE_LOOP ( 'NONE', ( #6187, #3241, #2022, #1591 ) ) ;
#4056 = DIRECTION ( 'NONE',  ( -1.000000000000000000, -0.000000000000000000, -0.000000000000000000 ) ) ;
#4057 = CARTESIAN_POINT ( 'NONE',  ( 2.000000000000000000, 1.773042676681340968, -2.276824562219559311E-15 ) ) ;
#4058 = DIRECTION ( 'NONE',  ( 0.000000000000000000, 0.000000000000000000, -1.000000000000000000 ) ) ;
#4059 = CARTESIAN_POINT ( 'NONE',  ( 0.1999999999999987899, 0.000000000000000000, 0.000000000000000000 ) ) ;
#4060 = CARTESIAN_POINT ( 'NONE',  ( 0.2500000000000002220, 4.898587196589412829E-16, -3.999999999999979128 ) ) ;
#4061 = CARTESIAN_POINT ( 'NONE',  ( -50.00000000000000000, 84.84335183244010636, -2.399999999999976374 ) ) ;
#4062 = DIRECTION ( 'NONE',  ( -1.000000000000000000, 0.000000000000000000, 0.000000000000000000 ) ) ;
#4063 = ORIENTED_EDGE ( 'NONE', *, *, #48, .F. ) ;
#4064 = EDGE_CURVE ( 'NONE', #3337, #2623, #443, .T. ) ;
#4065 = DIRECTION ( 'NONE',  ( 1.000000000000000000, 0.000000000000000000, -0.000000000000000000 ) ) ;
#4066 = AXIS2_PLACEMENT_3D ( 'NONE', #3805, #7135, #6328 ) ;
#4067 = ORIENTED_EDGE ( 'NONE', *, *, #5635, .T. ) ;
#4068 = VERTEX_POINT ( 'NONE', #6510 ) ;
#4069 = MANIFOLD_SOLID_BREP ( 'EndChamfer', #3846 ) ;
#4070 = LINE ( 'NONE', #7914, #7277 ) ;
#4071 = PLANE ( 'NONE',  #1228 ) ;
#4072 = CARTESIAN_POINT ( 'NONE',  ( 50.00000000000003553, 85.00000000000012790, -5.000000000000003553 ) ) ;
#4073 = DIRECTION ( 'NONE',  ( -0.000000000000000000, -0.000000000000000000, 1.000000000000000000 ) ) ;
#4074 = SHAPE_DEFINITION_REPRESENTATION ( #1802, #1314 ) ;
#4075 = ADVANCED_FACE ( 'NONE', ( #4535 ), #814, .T. ) ;
#4076 = ORIENTED_EDGE ( 'NONE', *, *, #3771, .F. ) ;
#4077 = EDGE_LOOP ( 'NONE', ( #5334, #7381, #7009, #4454 ) ) ;
#4078 = ORIENTED_EDGE ( 'NONE', *, *, #1809, .F. ) ;
#4079 = FACE_OUTER_BOUND ( 'NONE', #6981, .T. ) ;
#4080 = DIRECTION ( 'NONE',  ( 1.000000000000000000, 0.000000000000000000, 0.000000000000000000 ) ) ;
#4081 = CARTESIAN_POINT ( 'NONE',  ( 23.61000000000001364, 0.000000000000000000, 0.000000000000000000 ) ) ;
#4082 = AXIS2_PLACEMENT_3D ( 'NONE', #7706, #7080, #287 ) ;
#4083 = CIRCLE ( 'NONE', #3016, 2.500000000000000888 ) ;
#4084 = ADVANCED_FACE ( 'NONE', ( #3951 ), #7644, .F. ) ;
#4085 = VECTOR ( 'NONE', #6181, 1000.000000000000000 ) ;
#4086 = CIRCLE ( 'NONE', #2228, 1.280000000000000027 ) ;
#4087 = DIRECTION ( 'NONE',  ( 0.000000000000000000, 0.000000000000000000, 1.000000000000000000 ) ) ;
#4088 = FACE_OUTER_BOUND ( 'NONE', #2426, .T. ) ;
#4089 =( LENGTH_UNIT ( ) NAMED_UNIT ( * ) SI_UNIT ( .MILLI., .METRE. ) );
#4090 = CIRCLE ( 'NONE', #1856, 2.055000000000000160 ) ;
#4091 = DIRECTION ( 'NONE',  ( -1.000000000000000000, -0.000000000000000000, -0.000000000000000000 ) ) ;
#4092 = CLOSED_SHELL ( 'NONE', ( #7407, #2592, #445, #5310, #3719, #5469, #1714, #4442, #7344, #4209, #2681, #7194, #3385, #1785, #4715 ) ) ;
#4093 = AXIS2_PLACEMENT_3D ( 'NONE', #406, #6638, #2946 ) ;
#4094 = LINE ( 'NONE', #3386, #4954 ) ;
#4095 = AXIS2_PLACEMENT_3D ( 'NONE', #7802, #3405, #2739 ) ;
#4096 = VECTOR ( 'NONE', #4693, 1000.000000000000227 ) ;
#4097 = VERTEX_POINT ( 'NONE', #155 ) ;
#4098 = EDGE_LOOP ( 'NONE', ( #6157, #4911 ) ) ;
#4099 = CARTESIAN_POINT ( 'NONE',  ( -2.271448787322325728E-15, -4.618802153517061804, -2.700000000000000178 ) ) ;
#4100 = DIRECTION ( 'NONE',  ( 1.000000000000000000, 0.000000000000000000, 0.000000000000000000 ) ) ;
#4101 = DIRECTION ( 'NONE',  ( -1.000000000000000000, 0.000000000000000000, 0.000000000000000000 ) ) ;
#4102 = CARTESIAN_POINT ( 'NONE',  ( -41.96465185579608459, 86.73000941357497595, 1.682954651729597018 ) ) ;
#4103 = DIRECTION ( 'NONE',  ( -0.000000000000000000, -1.000000000000000000, -0.000000000000000000 ) ) ;
#4104 = DIRECTION ( 'NONE',  ( -1.000000000000000000, 0.000000000000000000, 0.000000000000000000 ) ) ;
#4105 = DIRECTION ( 'NONE',  ( 1.000000000000000000, 0.000000000000000000, 0.000000000000000000 ) ) ;
#4106 = ORIENTED_EDGE ( 'NONE', *, *, #4660, .F. ) ;
#4107 = DIRECTION ( 'NONE',  ( 0.000000000000000000, -0.4999999999999992784, 0.8660254037844390407 ) ) ;
#4108 = AXIS2_PLACEMENT_3D ( 'NONE', #3000, #8067, #2388 ) ;
#4109 = ORIENTED_EDGE ( 'NONE', *, *, #1541, .F. ) ;
#4110 = CONICAL_SURFACE ( 'NONE', #3985, 4.000000000000000000, 1.047197551196595855 ) ;
#4111 = ORIENTED_EDGE ( 'NONE', *, *, #6599, .F. ) ;
#4112 = MECHANICAL_DESIGN_GEOMETRIC_PRESENTATION_REPRESENTATION (  '', ( #7288 ), #3452 ) ;
#4113 = CARTESIAN_POINT ( 'NONE',  ( 30.00000000000000000, 0.000000000000000000, -6.938893903907228378E-15 ) ) ;
#4114 = DIRECTION ( 'NONE',  ( 0.000000000000000000, 0.000000000000000000, 1.000000000000000000 ) ) ;
#4115 = DIRECTION ( 'NONE',  ( 0.000000000000000000, 0.8660254037844379305, -0.5000000000000014433 ) ) ;
#4116 = CARTESIAN_POINT ( 'NONE',  ( -2.466926498672807888, 6.554919675146932079, 8.004187704512341739 ) ) ;
#4117 = EDGE_CURVE ( 'NONE', #6037, #5610, #2662, .T. ) ;
#4118 = DIRECTION ( 'NONE',  ( 0.000000000000000000, -1.000000000000000000, 1.320393690296331133E-15 ) ) ;
#4119 = APPLICATION_PROTOCOL_DEFINITION ( 'draft international standard', 'automotive_design', 1998, #7630 ) ;
#4120 = CIRCLE ( 'NONE', #3333, 7.000000000000000000 ) ;
#4121 = EDGE_LOOP ( 'NONE', ( #7178, #1896, #736, #6086 ) ) ;
#4122 = EDGE_LOOP ( 'NONE', ( #6830, #3905 ) ) ;
#4123 = ORIENTED_EDGE ( 'NONE', *, *, #4050, .F. ) ;
#4124 = DIRECTION ( 'NONE',  ( 1.000000000000000000, 0.000000000000000000, 0.000000000000000000 ) ) ;
#4125 = FACE_OUTER_BOUND ( 'NONE', #2782, .T. ) ;
#4126 = FACE_BOUND ( 'NONE', #1221, .T. ) ;
#4127 = VERTEX_POINT ( 'NONE', #5813 ) ;
#4128 = EDGE_CURVE ( 'NONE', #1429, #4916, #3421, .T. ) ;
#4129 = LINE ( 'NONE', #2838, #4511 ) ;
#4130 = CARTESIAN_POINT ( 'NONE',  ( -1.249999999999992673, 38.99999999999999289, -4.999999999999990230 ) ) ;
#4131 = PLANE ( 'NONE',  #3211 ) ;
#4132 = CYLINDRICAL_SURFACE ( 'NONE', #5874, 2.500000000000002220 ) ;
#4133 = AXIS2_PLACEMENT_3D ( 'NONE', #5492, #4115, #2786 ) ;
#4134 = ORIENTED_EDGE ( 'NONE', *, *, #50, .T. ) ;
#4135 = ORIENTED_EDGE ( 'NONE', *, *, #6839, .F. ) ;
#4136 = DIRECTION ( 'NONE',  ( -0.000000000000000000, -0.000000000000000000, 1.000000000000000000 ) ) ;
#4137 = DIRECTION ( 'NONE',  ( 1.000000000000000000, 0.000000000000000000, 0.000000000000000000 ) ) ;
#4138 = CARTESIAN_POINT ( 'NONE',  ( 0.000000000000000000, 0.000000000000000000, 8.000000000000000000 ) ) ;
#4139 = CARTESIAN_POINT ( 'NONE',  ( -41.99756812932358940, 85.51244622392444228, -2.358409241415399205 ) ) ;
#4140 = FACE_OUTER_BOUND ( 'NONE', #4803, .T. ) ;
#4141 = CARTESIAN_POINT ( 'NONE',  ( -49.99635120648662934, 84.37668793019695102, -2.322944911472436313 ) ) ;
#4142 = CIRCLE ( 'NONE', #7324, 1.649999999999984812 ) ;
#4143 = CARTESIAN_POINT ( 'NONE',  ( 39.83716857408421674, 108.0000000000001421, 4.163336342344337027E-14 ) ) ;
#4144 = ORIENTED_EDGE ( 'NONE', *, *, #7453, .F. ) ;
#4145 = CARTESIAN_POINT ( 'NONE',  ( 1.155036213957052500E-14, 4.618802153517020059, -2.700000000000000178 ) ) ;
#4146 = EDGE_LOOP ( 'NONE', ( #7368, #4106, #5410, #7728 ) ) ;
#4147 = EDGE_CURVE ( 'NONE', #2960, #5044, #7213, .T. ) ;
#4148 = ORIENTED_EDGE ( 'NONE', *, *, #6031, .F. ) ;
#4149 = EDGE_CURVE ( 'NONE', #2794, #5782, #4387, .T. ) ;
#4150 = DIRECTION ( 'NONE',  ( 0.000000000000000000, 0.000000000000000000, -1.000000000000000000 ) ) ;
#4151 = ADVANCED_FACE ( 'NONE', ( #5318 ), #1528, .F. ) ;
#4152 = DIRECTION ( 'NONE',  ( 1.000000000000000000, 0.000000000000000000, 0.000000000000000000 ) ) ;
#4153 = CARTESIAN_POINT ( 'NONE',  ( 2.500000000000002220, 1.178949249685212086, -2.042000000000002036 ) ) ;
#4154 = DIRECTION ( 'NONE',  ( -0.000000000000000000, 1.000000000000000000, -0.000000000000000000 ) ) ;
#4155 = CARTESIAN_POINT ( 'NONE',  ( -7.000000000000000000, 1.843750452292770530E-16, 8.033969604113661234 ) ) ;
#4156 = DIRECTION ( 'NONE',  ( 1.000000000000000000, -0.000000000000000000, -0.000000000000000000 ) ) ;
#4157 = SHAPE_DEFINITION_REPRESENTATION ( #6385, #6413 ) ;
#4158 = COLOUR_RGB ( '', 0.31764706, 0.68627451, 0.89019608) ;
#4159 = ORIENTED_EDGE ( 'NONE', *, *, #968, .T. ) ;
#4160 =( REPRESENTATION_RELATIONSHIP ('NONE','NONE', #3916, #7239 ) REPRESENTATION_RELATIONSHIP_WITH_TRANSFORMATION ( #2289 )SHAPE_REPRESENTATION_RELATIONSHIP( ) );
#4161 = ORIENTED_EDGE ( 'NONE', *, *, #5232, .F. ) ;
#4162 = ORIENTED_EDGE ( 'NONE', *, *, #3666, .T. ) ;
#4163 = DIRECTION ( 'NONE',  ( -0.000000000000000000, -0.000000000000000000, 1.000000000000000000 ) ) ;
#4164 = CARTESIAN_POINT ( 'NONE',  ( 0.000000000000000000, 0.8865213383406717051, 1.535499999999998533 ) ) ;
#4165 = DIRECTION ( 'NONE',  ( 1.000000000000000000, 0.000000000000000000, 0.000000000000000000 ) ) ;
#4166 = ORIENTED_EDGE ( 'NONE', *, *, #2876, .F. ) ;
#4167 = DIRECTION ( 'NONE',  ( -0.000000000000000000, -0.000000000000000000, 1.000000000000000000 ) ) ;
#4168 = EDGE_CURVE ( 'NONE', #3952, #1617, #6101, .T. ) ;
#4169 = LINE ( 'NONE', #1052, #238 ) ;
#4170 = CARTESIAN_POINT ( 'NONE',  ( 0.000000000000000000, 0.000000000000000000, 0.000000000000000000 ) ) ;
#4171 = CIRCLE ( 'NONE', #1796, 2.649999999999999467 ) ;
#4172 = PRODUCT_DEFINITION_SHAPE ( 'NONE', 'NONE',  #8214 ) ;
#4173 = ADVANCED_FACE ( 'NONE', ( #267 ), #4183, .F. ) ;
#4174 = CARTESIAN_POINT ( 'NONE',  ( -6.075269275428587967, -3.507208453717142849, 8.025542426815230002 ) ) ;
#4175 = CARTESIAN_POINT ( 'NONE',  ( 2.000000000000000000, 0.000000000000000000, 0.000000000000000000 ) ) ;
#4176 = ADVANCED_FACE ( 'NONE', ( #2815 ), #2387, .F. ) ;
#4177 = VERTEX_POINT ( 'NONE', #6712 ) ;
#4178 = ORIENTED_EDGE ( 'NONE', *, *, #1539, .T. ) ;
#4179 = CARTESIAN_POINT ( 'NONE',  ( 4.000000000000003553, 2.309401076758480720, -2.700000000000000178 ) ) ;
#4180 = DIRECTION ( 'NONE',  ( -0.000000000000000000, -0.000000000000000000, 1.000000000000000000 ) ) ;
#4181 = CARTESIAN_POINT ( 'NONE',  ( -41.93162413031724611, 87.39566059415857069, -0.1928755069452474658 ) ) ;
#4182 = PLANE ( 'NONE',  #4512 ) ;
#4183 = CYLINDRICAL_SURFACE ( 'NONE', #1335, 4.999999999999993783 ) ;
#4184 = CARTESIAN_POINT ( 'NONE',  ( -31.74999999999995737, 0.000000000000000000, 0.000000000000000000 ) ) ;
#4185 = EDGE_LOOP ( 'NONE', ( #6621, #7950, #4979 ) ) ;
#4186 = CARTESIAN_POINT ( 'NONE',  ( -2.650000000000003020, 0.000000000000000000, 10.00000000000000000 ) ) ;
#4187 = ORIENTED_EDGE ( 'NONE', *, *, #669, .T. ) ;
#4188 = ORIENTED_EDGE ( 'NONE', *, *, #5105, .T. ) ;
#4189 = CARTESIAN_POINT ( 'NONE',  ( 55.00000000000000000, -10.00000000000000000, 15.50000000000000355 ) ) ;
#4190 = DIRECTION ( 'NONE',  ( -0.7071067811865359154, 0.000000000000000000, 0.7071067811865591191 ) ) ;
#4191 = PLANE ( 'NONE',  #4133 ) ;
#4192 = DIRECTION ( 'NONE',  ( -1.000000000000000000, -0.000000000000000000, -0.000000000000000000 ) ) ;
#4193 = AXIS2_PLACEMENT_3D ( 'NONE', #872, #1512, #4047 ) ;
#4194 = CONTEXT_DEPENDENT_SHAPE_REPRESENTATION ( #6008, #4988 ) ;
#4195 = ORIENTED_EDGE ( 'NONE', *, *, #1276, .F. ) ;
#4196 = CONICAL_SURFACE ( 'NONE', #5266, 2.041999999999999815, 1.047197551196591858 ) ;
#4197 = ORIENTED_EDGE ( 'NONE', *, *, #8107, .T. ) ;
#4198 = CIRCLE ( 'NONE', #6990, 4.999999999999993783 ) ;
#4199 = EDGE_LOOP ( 'NONE', ( #6739, #2721 ) ) ;
#4200 = CARTESIAN_POINT ( 'NONE',  ( 1.270137496355039850E-14, 85.00000000000011369, 5.000000000000046185 ) ) ;
#4201 = DIRECTION ( 'NONE',  ( 1.412205397084881070E-17, -2.775557561562891967E-17, -1.000000000000000000 ) ) ;
#4202 = DIRECTION ( 'NONE',  ( 1.412205397084881070E-17, -2.775557561562891967E-17, -1.000000000000000000 ) ) ;
#4203 = SURFACE_STYLE_USAGE ( .BOTH. , #8056 ) ;
#4204 = EDGE_CURVE ( 'NONE', #6841, #6037, #1018, .T. ) ;
#4205 = ORIENTED_EDGE ( 'NONE', *, *, #4599, .F. ) ;
#4206 = CARTESIAN_POINT ( 'NONE',  ( -2.271448787322325728E-15, -4.618802153517061804, -2.700000000000000178 ) ) ;
#4207 = ORIENTED_EDGE ( 'NONE', *, *, #3542, .T. ) ;
#4208 = CYLINDRICAL_SURFACE ( 'NONE', #4108, 2.149999999999995470 ) ;
#4209 = ADVANCED_FACE ( 'NONE', ( #1567 ), #4766, .T. ) ;
#4210 = CARTESIAN_POINT ( 'NONE',  ( -38.58716857408418122, 108.0000000000001421, 4.165101599090693094E-14 ) ) ;
#4211 = FILL_AREA_STYLE_COLOUR ( '', #6225 ) ;
#4212 = ADVANCED_FACE ( 'NONE', ( #7993 ), #2005, .T. ) ;
#4213 = ADVANCED_FACE ( 'NONE', ( #3481 ), #6618, .T. ) ;
#4214 = UNCERTAINTY_MEASURE_WITH_UNIT (LENGTH_MEASURE( 1.000000000000000082E-05 ), #3467, 'distance_accuracy_value', 'NONE');
#4215 = FACE_OUTER_BOUND ( 'NONE', #5920, .T. ) ;
#4216 = AXIS2_PLACEMENT_3D ( 'NONE', #3478, #6002, #2472 ) ;
#4217 = ORIENTED_EDGE ( 'NONE', *, *, #5227, .T. ) ;
#4218 = VERTEX_POINT ( 'NONE', #1692 ) ;
#4219 = VECTOR ( 'NONE', #2827, 1000.000000000000000 ) ;
#4220 = CARTESIAN_POINT ( 'NONE',  ( 2.000000000000000000, 0.8865213383406717051, 1.535499999999998533 ) ) ;
#4221 = CARTESIAN_POINT ( 'NONE',  ( 50.00000000000000000, -10.00000000000000000, 0.000000000000000000 ) ) ;
#4222 = DIRECTION ( 'NONE',  ( -0.000000000000000000, -0.000000000000000000, 1.000000000000000000 ) ) ;
#4223 = APPLICATION_CONTEXT ( 'automotive_design' ) ;
#4224 = CARTESIAN_POINT ( 'NONE',  ( -49.96368263234898421, 83.09261300472543610, 1.465190138156000188 ) ) ;
#4225 = AXIS2_PLACEMENT_3D ( 'NONE', #4719, #7955, #3605 ) ;
#4226 = AXIS2_PLACEMENT_3D ( 'NONE', #824, #4696, #1501 ) ;
#4227 = DIRECTION ( 'NONE',  ( 1.000000000000000000, 0.000000000000000000, 0.000000000000000000 ) ) ;
#4228 = ORIENTED_EDGE ( 'NONE', *, *, #5618, .T. ) ;
#4229 = CARTESIAN_POINT ( 'NONE',  ( 1.250000000000003997, 38.99999999999999289, -1.765256746356099026E-17 ) ) ;
#4230 = ORIENTED_EDGE ( 'NONE', *, *, #6800, .T. ) ;
#4231 = ORIENTED_EDGE ( 'NONE', *, *, #111, .T. ) ;
#4232 = VECTOR ( 'NONE', #4190, 1000.000000000000000 ) ;
#4233 = CIRCLE ( 'NONE', #7687, 2.650000000000010125 ) ;
#4234 = CARTESIAN_POINT ( 'NONE',  ( 0.6554360035617808888, -4.240386000424090973, -0.1586754815285200126 ) ) ;
#4235 = VECTOR ( 'NONE', #6755, 1000.000000000000000 ) ;
#4236 = CARTESIAN_POINT ( 'NONE',  ( 1.250000000000004663, 38.99999999999999289, -4.999999999999990230 ) ) ;
#4237 = DIRECTION ( 'NONE',  ( -0.000000000000000000, 0.000000000000000000, -1.000000000000000000 ) ) ;
#4238 = EDGE_CURVE ( 'NONE', #5215, #6340, #3050, .T. ) ;
#4239 = CARTESIAN_POINT ( 'NONE',  ( -0.4613443011311406106, 7.000000000000005329, 8.000000000000021316 ) ) ;
#4240 = CARTESIAN_POINT ( 'NONE',  ( -1.600000000000004752, 42.68016229225776925, 4.000000000000000000 ) ) ;
#4241 = VECTOR ( 'NONE', #5749, 1000.000000000000000 ) ;
#4242 = CONTEXT_DEPENDENT_SHAPE_REPRESENTATION ( #2189, #4918 ) ;
#4243 = AXIS2_PLACEMENT_3D ( 'NONE', #4044, #2166, #4703 ) ;
#4244 = VECTOR ( 'NONE', #2064, 1000.000000000000000 ) ;
#4245 = ORIENTED_EDGE ( 'NONE', *, *, #2036, .F. ) ;
#4246 = VERTEX_POINT ( 'NONE', #3013 ) ;
#4247 = ORIENTED_EDGE ( 'NONE', *, *, #2323, .F. ) ;
#4248 = PRODUCT_DEFINITION_SHAPE ( 'NONE', 'NONE',  #2884 ) ;
#4249 = DIRECTION ( 'NONE',  ( -0.000000000000000000, 0.8660254037844391517, 0.4999999999999990563 ) ) ;
#4250 = CARTESIAN_POINT ( 'NONE',  ( 0.000000000000000000, 0.000000000000000000, 0.000000000000000000 ) ) ;
#4251 = TOROIDAL_SURFACE ( 'NONE', #670, 4.000000000000000000, 0.2500000000000000000 ) ;
#4252 = CARTESIAN_POINT ( 'NONE',  ( 40.00000000000000711, -39.99999999999999289, 0.000000000000000000 ) ) ;
#4253 = EDGE_LOOP ( 'NONE', ( #6174, #563 ) ) ;
#4254 = CARTESIAN_POINT ( 'NONE',  ( 55.00000000000000000, 10.00000000000000000, -2.849999999999991651 ) ) ;
#4255 = VECTOR ( 'NONE', #1361, 1000.000000000000000 ) ;
#4256 = EDGE_LOOP ( 'NONE', ( #4967, #5931 ) ) ;
#4257 = EDGE_LOOP ( 'NONE', ( #1407, #7999, #3449, #8061 ) ) ;
#4258 = EDGE_CURVE ( 'NONE', #4949, #402, #6215, .T. ) ;
#4259 = VECTOR ( 'NONE', #6661, 1000.000000000000000 ) ;
#4260 = CARTESIAN_POINT ( 'NONE',  ( -58.00000000000006395, -8.000000000000003553, 11.99999999999998934 ) ) ;
#4261 = EDGE_CURVE ( 'NONE', #1258, #3364, #4349, .T. ) ;
#4262 = CARTESIAN_POINT ( 'NONE',  ( -1.249999999999992228, 38.99999999999999289, -1.765256746356098409E-17 ) ) ;
#4263 = CARTESIAN_POINT ( 'NONE',  ( 1.599999999999986766, 37.49999999999999289, 4.000000000000001776 ) ) ;
#4264 = DIRECTION ( 'NONE',  ( 0.000000000000000000, -1.000000000000000000, 0.000000000000000000 ) ) ;
#4265 = ADVANCED_FACE ( 'NONE', ( #6927 ), #5062, .T. ) ;
#4266 = VERTEX_POINT ( 'NONE', #8127 ) ;
#4267 = VERTEX_POINT ( 'NONE', #4944 ) ;
#4268 = FILL_AREA_STYLE_COLOUR ( '', #2752 ) ;
#4269 = CARTESIAN_POINT ( 'NONE',  ( -31.74999999999994316, 0.000000000000000000, 0.000000000000000000 ) ) ;
#4270 = CARTESIAN_POINT ( 'NONE',  ( 24.00000000000000000, 0.000000000000000000, 0.000000000000000000 ) ) ;
#4271 = DIRECTION ( 'NONE',  ( 1.000000000000000000, 0.000000000000000000, 0.000000000000000000 ) ) ;
#4272 = CARTESIAN_POINT ( 'NONE',  ( -31.74999999999995737, 0.000000000000000000, 3.500000000000000000 ) ) ;
#4273 = CARTESIAN_POINT ( 'NONE',  ( -3.000000000000000888, 45.09008114612887397, 0.000000000000000000 ) ) ;
#4274 = ADVANCED_FACE ( 'NONE', ( #2440 ), #4985, .F. ) ;
#4275 = ORIENTED_EDGE ( 'NONE', *, *, #3229, .T. ) ;
#4276 = ADVANCED_FACE ( 'NONE', ( #4441, #1915 ), #8033, .F. ) ;
#4277 = ORIENTED_EDGE ( 'NONE', *, *, #8164, .T. ) ;
#4278 = DIRECTION ( 'NONE',  ( -0.000000000000000000, -0.000000000000000000, 1.000000000000000000 ) ) ;
#4279 = DIRECTION ( 'NONE',  ( -1.000000000000000000, -0.000000000000000000, -0.000000000000000000 ) ) ;
#4280 = FACE_OUTER_BOUND ( 'NONE', #7887, .T. ) ;
#4281 = CARTESIAN_POINT ( 'NONE',  ( 2.000000000000000000, 1.773042676681340968, -2.276824562219559311E-15 ) ) ;
#4282 = CARTESIAN_POINT ( 'NONE',  ( 9.020562070449730010E-14, 7.000000000000000000, 8.000000000000058620 ) ) ;
#4283 = FACE_OUTER_BOUND ( 'NONE', #5817, .T. ) ;
#4284 = EDGE_LOOP ( 'NONE', ( #2963, #3228, #229, #6053 ) ) ;
#4285 = EDGE_CURVE ( 'NONE', #5401, #1156, #3783, .T. ) ;
#4286 = EDGE_LOOP ( 'NONE', ( #2048, #2218, #1319 ) ) ;
#4287 = ORIENTED_EDGE ( 'NONE', *, *, #753, .F. ) ;
#4288 = ORIENTED_EDGE ( 'NONE', *, *, #1722, .T. ) ;
#4289 = CARTESIAN_POINT ( 'NONE',  ( 5.860087342385653250E-15, 38.99999999999999289, 0.000000000000000000 ) ) ;
#4290 = DIRECTION ( 'NONE',  ( 1.000000000000000000, 0.000000000000000000, 0.000000000000000000 ) ) ;
#4291 = DIRECTION ( 'NONE',  ( 0.000000000000000000, -0.000000000000000000, 1.000000000000000000 ) ) ;
#4292 = UNCERTAINTY_MEASURE_WITH_UNIT (LENGTH_MEASURE( 1.000000000000000082E-05 ), #2347, 'distance_accuracy_value', 'NONE');
#4293 = EDGE_LOOP ( 'NONE', ( #1965, #261, #5863, #6332 ) ) ;
#4294 = CARTESIAN_POINT ( 'NONE',  ( 4.000000000000002665, 1.557668341133515932, -0.1596965656957575197 ) ) ;
#4295 = ORIENTED_EDGE ( 'NONE', *, *, #174, .F. ) ;
#4296 = ORIENTED_EDGE ( 'NONE', *, *, #1241, .T. ) ;
#4297 = CARTESIAN_POINT ( 'NONE',  ( -4.999999999999997335, 6.123233995736758394E-16, 20.00000000000000355 ) ) ;
#4298 = CARTESIAN_POINT ( 'NONE',  ( 2.999999999999999112, 45.09008114612887397, 4.000000000000000000 ) ) ;
#4299 =( NAMED_UNIT ( * ) PLANE_ANGLE_UNIT ( ) SI_UNIT ( $, .RADIAN. ) );
#4300 = CARTESIAN_POINT ( 'NONE',  ( -6.765702216007799308, -1.810551654344674688, 8.031730529104347482 ) ) ;
#4301 = CARTESIAN_POINT ( 'NONE',  ( 3.099999999999998757, 0.000000000000000000, 0.000000000000000000 ) ) ;
#4302 = EDGE_CURVE ( 'NONE', #7783, #2623, #7422, .T. ) ;
#4303 = EDGE_CURVE ( 'NONE', #2014, #3623, #1240, .T. ) ;
#4304 = VERTEX_POINT ( 'NONE', #1145 ) ;
#4305 = ORIENTED_EDGE ( 'NONE', *, *, #3473, .F. ) ;
#4306 = CIRCLE ( 'NONE', #724, 1.649999999999995248 ) ;
#4307 = LINE ( 'NONE', #2480, #6589 ) ;
#4308 = CARTESIAN_POINT ( 'NONE',  ( -50.00000000000000711, 85.00000000000009948, 5.000000000000047073 ) ) ;
#4309 = FACE_OUTER_BOUND ( 'NONE', #6239, .T. ) ;
#4310 = DIRECTION ( 'NONE',  ( 0.000000000000000000, 0.000000000000000000, 1.000000000000000000 ) ) ;
#4311 = DIRECTION ( 'NONE',  ( -0.000000000000000000, 1.000000000000000000, -0.000000000000000000 ) ) ;
#4312 = FACE_BOUND ( 'NONE', #1122, .T. ) ;
#4313 = PRODUCT_DEFINITION_SHAPE ( 'NONE', 'NONE',  #6186 ) ;
#4314 = EDGE_LOOP ( 'NONE', ( #5601, #4456, #6248 ) ) ;
#4315 = VERTEX_POINT ( 'NONE', #524 ) ;
#4316 = DIRECTION ( 'NONE',  ( 1.412205397084881070E-17, -2.775557561562891967E-17, -1.000000000000000000 ) ) ;
#4317 = FACE_OUTER_BOUND ( 'NONE', #8052, .T. ) ;
#4318 = CARTESIAN_POINT ( 'NONE',  ( 20.00000000000000355, 1.971681346627238735E-16, -1.610000000000000098 ) ) ;
#4319 = CARTESIAN_POINT ( 'NONE',  ( -2.000000000000009770, 3.464101615137749057, -2.700000000000001066 ) ) ;
#4320 = DIRECTION ( 'NONE',  ( 0.000000000000000000, 0.000000000000000000, -1.000000000000000000 ) ) ;
#4321 = EDGE_CURVE ( 'NONE', #3296, #4618, #1467, .T. ) ;
#4322 = ADVANCED_FACE ( 'NONE', ( #6882, #6796 ), #3068, .T. ) ;
#4323 = DIRECTION ( 'NONE',  ( 0.000000000000000000, 0.000000000000000000, -1.000000000000000000 ) ) ;
#4324 = VERTEX_POINT ( 'NONE', #5687 ) ;
#4325 = ORIENTED_EDGE ( 'NONE', *, *, #6735, .T. ) ;
#4326 = ORIENTED_EDGE ( 'NONE', *, *, #4545, .F. ) ;
#4327 = VERTEX_POINT ( 'NONE', #7857 ) ;
#4328 = DIRECTION ( 'NONE',  ( 1.000000000000000000, 0.000000000000000000, 0.000000000000000000 ) ) ;
#4329 = CARTESIAN_POINT ( 'NONE',  ( 4.200000000000001954, 0.000000000000000000, 0.000000000000000000 ) ) ;
#4330 = LINE ( 'NONE', #587, #4749 ) ;
#4331 = ORIENTED_EDGE ( 'NONE', *, *, #7410, .F. ) ;
#4332 = FACE_OUTER_BOUND ( 'NONE', #3622, .T. ) ;
#4333 = CIRCLE ( 'NONE', #5267, 1.500000000000000222 ) ;
#4334 = ORIENTED_EDGE ( 'NONE', *, *, #7613, .F. ) ;
#4335 = B_SPLINE_CURVE_WITH_KNOTS ( 'NONE', 3,
 ( #3119, #1115, #5656, #1754, #4408, #5035 ),
 .UNSPECIFIED., .F., .F.,
 ( 4, 2, 4 ),
 ( 0.004120275011746842714, 0.005288420935197119671, 0.006456566858647395761 ),
 .UNSPECIFIED. ) ;
#4336 = ORIENTED_EDGE ( 'NONE', *, *, #7686, .T. ) ;
#4337 = FACE_BOUND ( 'NONE', #5503, .T. ) ;
#4338 = CARTESIAN_POINT ( 'NONE',  ( 3.999999999999999112, 0.000000000000000000, 0.000000000000000000 ) ) ;
#4339 = DIRECTION ( 'NONE',  ( -1.000000000000000000, -1.502586498047605218E-16, 1.238733049487200360E-17 ) ) ;
#4341 = EDGE_CURVE ( 'NONE', #1263, #4815, #6900, .T. ) ;
#4340 = SURFACE_STYLE_FILL_AREA ( #1229 ) ;
#4342 = CARTESIAN_POINT ( 'NONE',  ( 58.00000000000000000, 8.000000000000000000, 0.000000000000000000 ) ) ;
#4343 = CARTESIAN_POINT ( 'NONE',  ( 6.477744019519650287, 2.682274772516526351, 8.029074116683069917 ) ) ;
#4344 = EDGE_LOOP ( 'NONE', ( #5178, #3196, #3254, #1968 ) ) ;
#4345 = ORIENTED_EDGE ( 'NONE', *, *, #697, .F. ) ;
#4346 = SURFACE_STYLE_FILL_AREA ( #7463 ) ;
#4347 = CARTESIAN_POINT ( 'NONE',  ( 0.000000000000000000, -1.478016689125442706, 1.843143693225357538E-15 ) ) ;
#4348 = FACE_OUTER_BOUND ( 'NONE', #2832, .T. ) ;
#4349 = LINE ( 'NONE', #5023, #5193 ) ;
#4350 = DIRECTION ( 'NONE',  ( 1.000000000000000000, 0.000000000000000000, 0.000000000000000000 ) ) ;
#4351 = AXIS2_PLACEMENT_3D ( 'NONE', #4179, #7208, #4761 ) ;
#4352 = CARTESIAN_POINT ( 'NONE',  ( 2.000000000000000000, -1.773042676681340968, 2.059984127722458425E-15 ) ) ;
#4353 = VECTOR ( 'NONE', #1885, 1000.000000000000000 ) ;
#4354 = EDGE_LOOP ( 'NONE', ( #1573, #1173, #5720, #330 ) ) ;
#4355 = DIRECTION ( 'NONE',  ( 1.000000000000000000, 0.000000000000000000, 0.000000000000000000 ) ) ;
#4356 = EDGE_CURVE ( 'NONE', #1769, #3954, #2975, .T. ) ;
#4357 = CYLINDRICAL_SURFACE ( 'NONE', #1177, 7.000000000000000000 ) ;
#4358 = CARTESIAN_POINT ( 'NONE',  ( 30.00000000000001066, -29.99999999999997868, 10.00000000000000000 ) ) ;
#4359 = DIRECTION ( 'NONE',  ( -0.000000000000000000, -0.000000000000000000, 1.000000000000000000 ) ) ;
#4360 = AXIS2_PLACEMENT_3D ( 'NONE', #3078, #4409, #4488 ) ;
#4361 = CIRCLE ( 'NONE', #3970, 4.000000000000000000 ) ;
#4362 = LINE ( 'NONE', #3792, #7924 ) ;
#4363 = EDGE_CURVE ( 'NONE', #6955, #910, #1105, .T. ) ;
#4364 = CARTESIAN_POINT ( 'NONE',  ( 49.95662654559780691, 87.08399340104908504, -1.200635520122793620 ) ) ;
#4365 = ORIENTED_EDGE ( 'NONE', *, *, #222, .T. ) ;
#4366 = VECTOR ( 'NONE', #8106, 1000.000000000000000 ) ;
#4367 = CIRCLE ( 'NONE', #1987, 3.299999999999999822 ) ;
#4368 = AXIS2_PLACEMENT_3D ( 'NONE', #6171, #476, #3866 ) ;
#4369 = VERTEX_POINT ( 'NONE', #3741 ) ;
#4370 = CIRCLE ( 'NONE', #2241, 0.2500000000000002220 ) ;
#4371 = EDGE_CURVE ( 'NONE', #7330, #939, #8074, .T. ) ;
#4372 = VECTOR ( 'NONE', #4278, 1000.000000000000000 ) ;
#4373 = ORIENTED_EDGE ( 'NONE', *, *, #7250, .T. ) ;
#4374 = ORIENTED_EDGE ( 'NONE', *, *, #6916, .T. ) ;
#4375 = FACE_OUTER_BOUND ( 'NONE', #7841, .T. ) ;
#4376 = DIRECTION ( 'NONE',  ( 0.000000000000000000, 0.000000000000000000, -1.000000000000000000 ) ) ;
#4377 = CARTESIAN_POINT ( 'NONE',  ( 11.00000000000000355, 0.000000000000000000, 0.000000000000000000 ) ) ;
#4378 = AXIS2_PLACEMENT_3D ( 'NONE', #3728, #5470, #3676 ) ;
#4379 = DIRECTION ( 'NONE',  ( 1.000000000000000000, 0.000000000000000000, 0.000000000000000000 ) ) ;
#4380 = AXIS2_PLACEMENT_3D ( 'NONE', #2390, #7456, #4838 ) ;
#4381 = EDGE_LOOP ( 'NONE', ( #961, #5333, #8090, #5000, #3 ) ) ;
#4382 = DIRECTION ( 'NONE',  ( -1.000000000000000000, -0.000000000000000000, -0.000000000000000000 ) ) ;
#4383 = AXIS2_PLACEMENT_3D ( 'NONE', #477, #2403, #4945 ) ;
#4384 = ORIENTED_EDGE ( 'NONE', *, *, #3763, .F. ) ;
#4385 = ORIENTED_EDGE ( 'NONE', *, *, #3219, .F. ) ;
#4386 = AXIS2_PLACEMENT_3D ( 'NONE', #7068, #3086, #6 ) ;
#4387 = CIRCLE ( 'NONE', #249, 2.149999999999999023 ) ;
#4388 = CARTESIAN_POINT ( 'NONE',  ( 0.000000000000000000, -0.7390083445627200209, 1.280000000000001137 ) ) ;
#4389 = DIRECTION ( 'NONE',  ( -1.000000000000000000, -0.000000000000000000, -0.000000000000000000 ) ) ;
#4390 = CARTESIAN_POINT ( 'NONE',  ( 55.00000000000000000, -8.000000000000001776, 15.50000000000000355 ) ) ;
#4391 = SURFACE_STYLE_USAGE ( .BOTH. , #3142 ) ;
#4392 = AXIS2_PLACEMENT_3D ( 'NONE', #3193, #641, #3858 ) ;
#4393 = EDGE_CURVE ( 'NONE', #4714, #6596, #2770, .T. ) ;
#4394 = AXIS2_PLACEMENT_3D ( 'NONE', #831, #5257, #5945 ) ;
#4395 = CARTESIAN_POINT ( 'NONE',  ( 6.067105206393708094, 3.498950914359637121, 8.025510423632917778 ) ) ;
#4396 = AXIS2_PLACEMENT_3D ( 'NONE', #4638, #2880, #5383 ) ;
#4397 = ORIENTED_EDGE ( 'NONE', *, *, #2354, .F. ) ;
#4398 = ORIENTED_EDGE ( 'NONE', *, *, #1667, .T. ) ;
#4399 = CARTESIAN_POINT ( 'NONE',  ( 4.000000000000004441, -1.549102112939112486, -0.1578953385959447620 ) ) ;
#4400 = LINE ( 'NONE', #7548, #1704 ) ;
#4401 = DIRECTION ( 'NONE',  ( 0.000000000000000000, 0.000000000000000000, 1.000000000000000000 ) ) ;
#4402 = CARTESIAN_POINT ( 'NONE',  ( -4.999999999999993783, 0.000000000000000000, 0.000000000000000000 ) ) ;
#4403 = FACE_OUTER_BOUND ( 'NONE', #4418, .T. ) ;
#4404 = CARTESIAN_POINT ( 'NONE',  ( 0.000000000000000000, 0.000000000000000000, 0.000000000000000000 ) ) ;
#4405 = ORIENTED_EDGE ( 'NONE', *, *, #1159, .F. ) ;
#4406 = DIRECTION ( 'NONE',  ( 0.000000000000000000, 1.000000000000000000, 0.000000000000000000 ) ) ;
#4407 = DIRECTION ( 'NONE',  ( -1.000000000000000000, -0.000000000000000000, -0.000000000000000000 ) ) ;
#4408 = CARTESIAN_POINT ( 'NONE',  ( -4.000000000000000000, -0.3902508023145541127, 1.101142831430590133E-17 ) ) ;
#4409 = DIRECTION ( 'NONE',  ( -0.000000000000000000, -0.000000000000000000, 1.000000000000000000 ) ) ;
#4410 = CARTESIAN_POINT ( 'NONE',  ( 2.681483223904246316, -3.070647092368467668, -2.032850044890171669E-14 ) ) ;
#4411 = ORIENTED_EDGE ( 'NONE', *, *, #1506, .F. ) ;
#4412 = ADVANCED_FACE ( 'NONE', ( #2575 ), #7635, .T. ) ;
#4413 = EDGE_CURVE ( 'NONE', #2734, #5289, #3201, .T. ) ;
#4414 = ORIENTED_EDGE ( 'NONE', *, *, #5661, .T. ) ;
#4415 = EDGE_CURVE ( 'NONE', #5903, #8200, #2903, .T. ) ;
#4416 = DIRECTION ( 'NONE',  ( 0.000000000000000000, 0.4999999999999990008, -0.8660254037844391517 ) ) ;
#4417 = PRODUCT_DEFINITION_CONTEXT ( 'detailed design', #4503, 'design' ) ;
#4418 = EDGE_LOOP ( 'NONE', ( #2933, #7523, #2190, #4464 ) ) ;
#4419 = ORIENTED_EDGE ( 'NONE', *, *, #7795, .T. ) ;
#4420 = DIRECTION ( 'NONE',  ( -0.000000000000000000, -0.000000000000000000, -1.000000000000000000 ) ) ;
#4421 = LINE ( 'NONE', #6947, #1342 ) ;
#4422 = CARTESIAN_POINT ( 'NONE',  ( 2.500000000000002220, -2.357898499370430834, 3.469446951953614189E-15 ) ) ;
#4423 = DIRECTION ( 'NONE',  ( 6.123233995736766036E-17, 1.363075293218192124E-18, -1.000000000000000000 ) ) ;
#4424 = CIRCLE ( 'NONE', #3896, 1.599999999999986766 ) ;
#4425 = ORIENTED_EDGE ( 'NONE', *, *, #7826, .T. ) ;
#4426 = CARTESIAN_POINT ( 'NONE',  ( 49.95669240716474491, 82.91758674606779778, 1.203334160065640646 ) ) ;
#4427 = ORIENTED_EDGE ( 'NONE', *, *, #6931, .F. ) ;
#4428 = VERTEX_POINT ( 'NONE', #5654 ) ;
#4429 = DIRECTION ( 'NONE',  ( -0.7071067811865310304, 8.659560562355135004E-17, -0.7071067811865641151 ) ) ;
#4430 = CARTESIAN_POINT ( 'NONE',  ( 41.93694813901194607, 82.69907418281616174, 0.6942729367014212061 ) ) ;
#4431 = DIRECTION ( 'NONE',  ( 0.000000000000000000, 1.103561164596346103E-15, 1.000000000000000000 ) ) ;
#4432 = VERTEX_POINT ( 'NONE', #6391 ) ;
#4433 = CARTESIAN_POINT ( 'NONE',  ( 60.00000000000000711, 9.332579536216795825E-15, 54.99999999999997868 ) ) ;
#4434 = CARTESIAN_POINT ( 'NONE',  ( 1.300000000000000044, -1.478016689125442706, 1.843143693225357538E-15 ) ) ;
#4435 = MECHANICAL_DESIGN_GEOMETRIC_PRESENTATION_REPRESENTATION (  '', ( #1510 ), #436 ) ;
#4436 = ORIENTED_EDGE ( 'NONE', *, *, #6594, .F. ) ;
#4437 = VERTEX_POINT ( 'NONE', #4558 ) ;
#4438 = FACE_OUTER_BOUND ( 'NONE', #8111, .T. ) ;
#4439 = CARTESIAN_POINT ( 'NONE',  ( -58.00000000000006395, -8.000000000000003553, 11.99999999999998934 ) ) ;
#4440 = DIRECTION ( 'NONE',  ( -1.000000000000000000, -0.000000000000000000, -0.000000000000000000 ) ) ;
#4441 = FACE_BOUND ( 'NONE', #7416, .T. ) ;
#4442 = ADVANCED_FACE ( 'NONE', ( #5572, #726 ), #6270, .F. ) ;
#4443 = FACE_BOUND ( 'NONE', #490, .T. ) ;
#4444 = DIRECTION ( 'NONE',  ( 0.000000000000000000, 0.000000000000000000, 1.000000000000000000 ) ) ;
#4445 = AXIS2_PLACEMENT_3D ( 'NONE', #3514, #974, #2888 ) ;
#4446 = VERTEX_POINT ( 'NONE', #1830 ) ;
#4447 = LINE ( 'NONE', #3829, #6023 ) ;
#4448 = PLANE ( 'NONE',  #5042 ) ;
#4449 = DIRECTION ( 'NONE',  ( 0.000000000000000000, 0.000000000000000000, 1.000000000000000000 ) ) ;
#4450 = DIRECTION ( 'NONE',  ( -1.412205397084881070E-17, 2.775557561562891967E-17, 1.000000000000000000 ) ) ;
#4451 = DIRECTION ( 'NONE',  ( -1.000000000000000000, -0.000000000000000000, -0.000000000000000000 ) ) ;
#4452 = ADVANCED_FACE ( 'NONE', ( #4317 ), #4991, .F. ) ;
#4453 = VERTEX_POINT ( 'NONE', #5194 ) ;
#4454 = ORIENTED_EDGE ( 'NONE', *, *, #404, .F. ) ;
#4455 = DIRECTION ( 'NONE',  ( 0.000000000000000000, 1.000000000000000000, 0.000000000000000000 ) ) ;
#4456 = ORIENTED_EDGE ( 'NONE', *, *, #1128, .F. ) ;
#4457 = EDGE_LOOP ( 'NONE', ( #3036, #4843, #7731 ) ) ;
#4458 = LINE ( 'NONE', #6906, #1988 ) ;
#4459 = LINE ( 'NONE', #3176, #3867 ) ;
#4460 = DIRECTION ( 'NONE',  ( 0.000000000000000000, 0.000000000000000000, 1.000000000000000000 ) ) ;
#4461 = EDGE_CURVE ( 'NONE', #1258, #397, #6653, .T. ) ;
#4462 = CARTESIAN_POINT ( 'NONE',  ( -1.137226034424574155E-15, 45.61196202519845855, 2.671627574707655623E-17 ) ) ;
#4463 = ORIENTED_EDGE ( 'NONE', *, *, #2391, .T. ) ;
#4464 = ORIENTED_EDGE ( 'NONE', *, *, #2444, .F. ) ;
#4465 = VERTEX_POINT ( 'NONE', #3269 ) ;
#4466 = DIRECTION ( 'NONE',  ( -1.000000000000000000, -0.000000000000000000, -0.000000000000000000 ) ) ;
#4467 = CARTESIAN_POINT ( 'NONE',  ( 41.97907998747123770, 86.32940376908055669, -2.002229301367421055 ) ) ;
#4468 = CARTESIAN_POINT ( 'NONE',  ( -25.00000000000000711, -29.99999999999999289, 10.00000000000000000 ) ) ;
#4469 =( NAMED_UNIT ( * ) SI_UNIT ( $, .STERADIAN. ) SOLID_ANGLE_UNIT ( ) );
#4470 = VECTOR ( 'NONE', #3397, 1000.000000000000000 ) ;
#4471 = CARTESIAN_POINT ( 'NONE',  ( -1.588954872702794896, -6.821165568473427143, 8.001714880650744988 ) ) ;
#4472 = EDGE_CURVE ( 'NONE', #554, #3168, #511, .T. ) ;
#4473 = ORIENTED_EDGE ( 'NONE', *, *, #7613, .T. ) ;
#4474 = AXIS2_PLACEMENT_3D ( 'NONE', #3557, #304, #887 ) ;
#4475 = AXIS2_PLACEMENT_3D ( 'NONE', #4987, #3688, #3611 ) ;
#4476 = ADVANCED_FACE ( 'NONE', ( #1403 ), #4357, .F. ) ;
#4477 = CARTESIAN_POINT ( 'NONE',  ( 58.00000000000000000, 8.000000000000000000, -8.000000000000000000 ) ) ;
#4478 = LINE ( 'NONE', #4347, #645 ) ;
#4479 = LINE ( 'NONE', #6500, #1455 ) ;
#4480 = DIRECTION ( 'NONE',  ( -0.5000000000000034417, 0.000000000000000000, 0.8660254037844367092 ) ) ;
#4481 = EDGE_CURVE ( 'NONE', #590, #2562, #3656, .T. ) ;
#4482 = DIRECTION ( 'NONE',  ( 0.000000000000000000, 0.000000000000000000, 1.000000000000000000 ) ) ;
#4483 = CARTESIAN_POINT ( 'NONE',  ( -49.94237310791755391, 87.39986840612061769, -0.1602877778557319222 ) ) ;
#4484 = ORIENTED_EDGE ( 'NONE', *, *, #2736, .T. ) ;
#4485 = CARTESIAN_POINT ( 'NONE',  ( 32.65000000000000568, -29.99999999999997868, 4.599999999999997868 ) ) ;
#4486 = DIRECTION ( 'NONE',  ( 0.000000000000000000, -1.000000000000000000, 0.000000000000000000 ) ) ;
#4487 = AXIS2_PLACEMENT_3D ( 'NONE', #6383, #7042, #1269 ) ;
#4488 = DIRECTION ( 'NONE',  ( 1.000000000000000000, 0.000000000000000000, 0.000000000000000000 ) ) ;
#4489 = CARTESIAN_POINT ( 'NONE',  ( 0.000000000000000000, -0.7390083445627200209, 1.280000000000001137 ) ) ;
#4490 = CIRCLE ( 'NONE', #1839, 721.2499999999977263 ) ;
#4491 = ORIENTED_EDGE ( 'NONE', *, *, #1634, .F. ) ;
#4492 = ORIENTED_EDGE ( 'NONE', *, *, #2119, .T. ) ;
#4493 = DIRECTION ( 'NONE',  ( 0.000000000000000000, 0.000000000000000000, -1.000000000000000000 ) ) ;
#4494 = AXIS2_PLACEMENT_3D ( 'NONE', #1411, #2112, #4645 ) ;
#4495 = ORIENTED_EDGE ( 'NONE', *, *, #4302, .T. ) ;
#4496 = EDGE_CURVE ( 'NONE', #2291, #550, #4951, .T. ) ;
#4497 = ORIENTED_EDGE ( 'NONE', *, *, #1582, .T. ) ;
#4498 = DIRECTION ( 'NONE',  ( 1.000000000000000000, 0.000000000000000000, 0.000000000000000000 ) ) ;
#4499 = DIRECTION ( 'NONE',  ( -0.000000000000000000, 1.000000000000000000, -0.000000000000000000 ) ) ;
#4500 = CARTESIAN_POINT ( 'NONE',  ( -1.198153218366585720E-14, 42.68016229225776925, 0.000000000000000000 ) ) ;
#4501 = CARTESIAN_POINT ( 'NONE',  ( 5.099239104286152439E-16, 18.71196202519845997, -9.950449640492676279E-18 ) ) ;
#4502 = AXIS2_PLACEMENT_3D ( 'NONE', #1424, #2742, #5938 ) ;
#4503 = APPLICATION_CONTEXT ( 'automotive_design' ) ;
#4504 = VECTOR ( 'NONE', #5282, 1000.000000000000000 ) ;
#4505 = AXIS2_PLACEMENT_3D ( 'NONE', #26, #2573, #5768 ) ;
#4506 = VECTOR ( 'NONE', #3620, 1000.000000000000000 ) ;
#4507 = ORIENTED_EDGE ( 'NONE', *, *, #3750, .T. ) ;
#4508 = VERTEX_POINT ( 'NONE', #1205 ) ;
#4509 = ORIENTED_EDGE ( 'NONE', *, *, #4545, .T. ) ;
#4510 = AXIS2_PLACEMENT_3D ( 'NONE', #4565, #7094, #7172 ) ;
#4511 = VECTOR ( 'NONE', #4019, 1000.000000000000000 ) ;
#4513 = DIRECTION ( 'NONE',  ( 0.000000000000000000, 0.000000000000000000, -1.000000000000000000 ) ) ;
#4512 = AXIS2_PLACEMENT_3D ( 'NONE', #3606, #6579, #6134 ) ;
#4514 = CARTESIAN_POINT ( 'NONE',  ( 41.93161960896016893, 87.39568130184227357, 0.1926422142524573111 ) ) ;
#4515 = FACE_OUTER_BOUND ( 'NONE', #4774, .T. ) ;
#4516 = CARTESIAN_POINT ( 'NONE',  ( 0.000000000000000000, 0.000000000000000000, 8.000000000000000000 ) ) ;
#4517 = VECTOR ( 'NONE', #4830, 1000.000000000000000 ) ;
#4518 = ADVANCED_FACE ( 'NONE', ( #2063, #4593 ), #6844, .F. ) ;
#4519 = CIRCLE ( 'NONE', #525, 4.999999999999993783 ) ;
#4520 = EDGE_CURVE ( 'NONE', #6955, #7075, #1113, .T. ) ;
#4521 = CARTESIAN_POINT ( 'NONE',  ( -24.99999999999999289, 30.00000000000000711, 4.599999999999997868 ) ) ;
#4522 = DIRECTION ( 'NONE',  ( 0.000000000000000000, -1.000000000000000000, 0.000000000000000000 ) ) ;
#4523 = DIRECTION ( 'NONE',  ( -1.000000000000000000, -0.000000000000000000, -0.000000000000000000 ) ) ;
#4524 = DIRECTION ( 'NONE',  ( -1.000000000000000000, 0.000000000000000000, 0.000000000000000000 ) ) ;
#4525 = AXIS2_PLACEMENT_3D ( 'NONE', #7929, #172, #2254 ) ;
#4526 = CARTESIAN_POINT ( 'NONE',  ( 29.99999999999997868, 30.00000000000001421, 10.00000000000000000 ) ) ;
#4527 = EDGE_CURVE ( 'NONE', #7545, #4446, #1859, .T. ) ;
#4528 = CARTESIAN_POINT ( 'NONE',  ( -49.94311118432959518, 87.38465289139489300, 0.3128412141715384842 ) ) ;
#4529 = CIRCLE ( 'NONE', #4392, 1.535500000000000087 ) ;
#4530 = VERTEX_POINT ( 'NONE', #4521 ) ;
#4531 = DIRECTION ( 'NONE',  ( 1.412205397084881070E-17, -2.775557561562891967E-17, -1.000000000000000000 ) ) ;
#4532 = FACE_OUTER_BOUND ( 'NONE', #5861, .T. ) ;
#4533 = DIRECTION ( 'NONE',  ( 0.000000000000000000, 0.000000000000000000, 1.000000000000000000 ) ) ;
#4534 = LINE ( 'NONE', #6463, #2895 ) ;
#4535 = FACE_OUTER_BOUND ( 'NONE', #6009, .T. ) ;
#4536 = ADVANCED_FACE ( 'NONE', ( #5846 ), #7275, .F. ) ;
#4537 = ORIENTED_EDGE ( 'NONE', *, *, #4793, .F. ) ;
#4538 = EDGE_CURVE ( 'NONE', #604, #3524, #575, .T. ) ;
#4539 = VERTEX_POINT ( 'NONE', #483 ) ;
#4540 = CARTESIAN_POINT ( 'NONE',  ( -4.000000000000000000, -1.933795701539609668, -2.451162342337703137 ) ) ;
#4541 = EDGE_LOOP ( 'NONE', ( #106, #6315, #2460, #3138, #7493 ) ) ;
#4542 = ORIENTED_EDGE ( 'NONE', *, *, #1750, .F. ) ;
#4543 = CARTESIAN_POINT ( 'NONE',  ( -38.58716857408418122, 108.0000000000001421, 4.161571085597980959E-14 ) ) ;
#4545 = EDGE_CURVE ( 'NONE', #2202, #8104, #2409, .T. ) ;
#4544 = CARTESIAN_POINT ( 'NONE',  ( -30.00000000000000355, -29.99999999999999289, 4.599999999999997868 ) ) ;
#4546 = CARTESIAN_POINT ( 'NONE',  ( 2.060000000000000941, 0.000000000000000000, -0.3080913168122707546 ) ) ;
#4547 = DIRECTION ( 'NONE',  ( -4.190029316300625537E-17, -2.493537746491834331E-17, 1.000000000000000000 ) ) ;
#4548 = ORIENTED_EDGE ( 'NONE', *, *, #6208, .F. ) ;
#4549 = VECTOR ( 'NONE', #7959, 1000.000000000000000 ) ;
#4550 = ORIENTED_EDGE ( 'NONE', *, *, #4027, .F. ) ;
#4551 = ORIENTED_EDGE ( 'NONE', *, *, #621, .T. ) ;
#4552 = DIRECTION ( 'NONE',  ( -0.000000000000000000, 1.000000000000000000, -0.000000000000000000 ) ) ;
#4553 = CARTESIAN_POINT ( 'NONE',  ( 41.98244464128908504, 86.21953388413311359, -2.071021427375734358 ) ) ;
#4554 = CYLINDRICAL_SURFACE ( 'NONE', #1693, 1.599999999999992983 ) ;
#4555 = CIRCLE ( 'NONE', #5991, 1.280000000000000027 ) ;
#4556 = SHAPE_REPRESENTATION_RELATIONSHIP ( 'NONE' , 'NONE' ,  #7239, #886 ) ;
#4557 = FACE_OUTER_BOUND ( 'NONE', #3401, .T. ) ;
#4558 = CARTESIAN_POINT ( 'NONE',  ( -32.64999999999999858, -29.99999999999999289, 4.599999999999997868 ) ) ;
#4559 = CARTESIAN_POINT ( 'NONE',  ( 10.00000000000000000, 1.224646799147353256E-15, 10.00000000000000000 ) ) ;
#4560 = LINE ( 'NONE', #805, #120 ) ;
#4561 = DIRECTION ( 'NONE',  ( 1.000000000000000000, 0.000000000000000000, -0.000000000000000000 ) ) ;
#4562 = DIRECTION ( 'NONE',  ( -0.000000000000000000, -0.000000000000000000, 1.000000000000000000 ) ) ;
#4563 = VERTEX_POINT ( 'NONE', #8168 ) ;
#4564 = CARTESIAN_POINT ( 'NONE',  ( 2.500000000000002220, 0.000000000000000000, -2.700000000000001066 ) ) ;
#4565 = CARTESIAN_POINT ( 'NONE',  ( -52.00000000000006395, -8.000000000000003553, 11.99999999999998934 ) ) ;
#4566 = CARTESIAN_POINT ( 'NONE',  ( 52.00000000000000711, -8.000000000000000000, 0.000000000000000000 ) ) ;
#4567 = AXIS2_PLACEMENT_3D ( 'NONE', #1895, #1973, #3291 ) ;
#4568 = DIRECTION ( 'NONE',  ( 1.412205397084881070E-17, -2.775557561562891967E-17, -1.000000000000000000 ) ) ;
#4569 = CARTESIAN_POINT ( 'NONE',  ( 4.000000000000003553, 2.309401076758524685, -0.3572655899081733644 ) ) ;
#4570 = VERTEX_POINT ( 'NONE', #2488 ) ;
#4571 = LINE ( 'NONE', #6861, #6451 ) ;
#4572 = PRODUCT_DEFINITION_FORMATION_WITH_SPECIFIED_SOURCE ( 'ANY', '', #7499, .NOT_KNOWN. ) ;
#4573 = ORIENTED_EDGE ( 'NONE', *, *, #7218, .T. ) ;
#4574 = PLANE ( 'NONE',  #5189 ) ;
#4575 = EDGE_LOOP ( 'NONE', ( #3277, #2526, #4325, #1089, #3709 ) ) ;
#4576 = ORIENTED_EDGE ( 'NONE', *, *, #7323, .T. ) ;
#4577 = ADVANCED_FACE ( 'NONE', ( #2450 ), #1990, .F. ) ;
#4578 = EDGE_CURVE ( 'NONE', #7025, #4304, #4747, .T. ) ;
#4579 = CYLINDRICAL_SURFACE ( 'NONE', #1170, 1.250000000000001110 ) ;
#4580 = VECTOR ( 'NONE', #4406, 1000.000000000000000 ) ;
#4581 = EDGE_CURVE ( 'NONE', #3093, #2553, #2514, .T. ) ;
#4582 = DIRECTION ( 'NONE',  ( 0.000000000000000000, -1.000000000000000000, 9.783878858594330870E-16 ) ) ;
#4583 = DIRECTION ( 'NONE',  ( -0.9803631929825737945, 0.1972004306410427010, -1.474514954580286030E-17 ) ) ;
#4584 = VERTEX_POINT ( 'NONE', #5343 ) ;
#4585 = VERTEX_POINT ( 'NONE', #2172 ) ;
#4586 = ORIENTED_EDGE ( 'NONE', *, *, #7483, .T. ) ;
#4587 = DIRECTION ( 'NONE',  ( -1.000000000000000000, -0.000000000000000000, -0.000000000000000000 ) ) ;
#4588 = CARTESIAN_POINT ( 'NONE',  ( 0.1999999999999987899, 4.041334437186265510E-16, -3.299999999999999822 ) ) ;
#4589 = CARTESIAN_POINT ( 'NONE',  ( 40.00000000000000711, 40.00000000000000711, 10.00000000000000000 ) ) ;
#4590 = FILL_AREA_STYLE ('',( #2568 ) ) ;
#4591 = DIRECTION ( 'NONE',  ( -1.000000000000000000, 0.000000000000000000, 0.000000000000000000 ) ) ;
#4592 = EDGE_CURVE ( 'NONE', #7111, #7104, #6217, .T. ) ;
#4593 = FACE_OUTER_BOUND ( 'NONE', #1356, .T. ) ;
#4594 = CYLINDRICAL_SURFACE ( 'NONE', #6093, 10.00000000000000000 ) ;
#4595 = AXIS2_PLACEMENT_3D ( 'NONE', #3672, #503, #3044 ) ;
#4596 =( LENGTH_UNIT ( ) NAMED_UNIT ( * ) SI_UNIT ( .MILLI., .METRE. ) );
#4597 = FACE_BOUND ( 'NONE', #411, .T. ) ;
#4598 = CARTESIAN_POINT ( 'NONE',  ( -49.96747517473576750, 86.80656978053563932, -1.587697219280529648 ) ) ;
#4599 = EDGE_CURVE ( 'NONE', #2407, #5094, #7198, .T. ) ;
#4600 = CONICAL_SURFACE ( 'NONE', #2083, 4.000000000000000000, 1.047197551196595855 ) ;
#4601 = AXIS2_PLACEMENT_3D ( 'NONE', #399, #2942, #2316 ) ;
#4602 = VERTEX_POINT ( 'NONE', #7235 ) ;
#4603 = PLANE ( 'NONE',  #2843 ) ;
#4604 = CARTESIAN_POINT ( 'NONE',  ( 57.99999999999999289, -8.000000000000003553, 11.99999999999998934 ) ) ;
#4605 = CARTESIAN_POINT ( 'NONE',  ( 0.1999999999999987899, 0.000000000000000000, 3.299999999999999822 ) ) ;
#4606 = FACE_OUTER_BOUND ( 'NONE', #1101, .T. ) ;
#4607 = CARTESIAN_POINT ( 'NONE',  ( -49.98571321592396544, 83.79770962390497857, 2.083050663831744309 ) ) ;
#4608 = ORIENTED_EDGE ( 'NONE', *, *, #1826, .F. ) ;
#4609 = CARTESIAN_POINT ( 'NONE',  ( 49.94312129582970528, 82.61555530433814454, 0.3147289805185609635 ) ) ;
#4610 = EDGE_LOOP ( 'NONE', ( #6598, #4608, #4197, #2024 ) ) ;
#4611 = ADVANCED_FACE ( 'NONE', ( #2263 ), #516, .F. ) ;
#4612 = EDGE_LOOP ( 'NONE', ( #5447, #7305, #8092, #747 ) ) ;
#4613 = VERTEX_POINT ( 'NONE', #5421 ) ;
#4614 = DIRECTION ( 'NONE',  ( -1.000000000000000000, 1.776356839400250465E-15, 0.000000000000000000 ) ) ;
#4615 = CARTESIAN_POINT ( 'NONE',  ( 0.000000000000000000, -0.7390083445627225744, -1.279999999999999138 ) ) ;
#4616 = SHAPE_DEFINITION_REPRESENTATION ( #7426, #1368 ) ;
#4617 = COLOUR_RGB ( '', 0.66274510, 0.83137255, 0.94901961) ;
#4618 = VERTEX_POINT ( 'NONE', #332 ) ;
#4619 = EDGE_LOOP ( 'NONE', ( #2021, #4723, #3284, #1294 ) ) ;
#4620 = EDGE_LOOP ( 'NONE', ( #2298, #7340 ) ) ;
#4621 = PRESENTATION_LAYER_ASSIGNMENT (  '', '', ( #8195 ) ) ;
#4622 = PLANE ( 'NONE',  #3579 ) ;
#4623 = CARTESIAN_POINT ( 'NONE',  ( 7.000000000000000000, 8.572527785734883977E-16, 8.033969604113771368 ) ) ;
#4624 = DIRECTION ( 'NONE',  ( 0.000000000000000000, 0.000000000000000000, 1.000000000000000000 ) ) ;
#4625 = CIRCLE ( 'NONE', #3303, 3.500000000000000000 ) ;
#4626 = VECTOR ( 'NONE', #7183, 1000.000000000000114 ) ;
#4627 = SURFACE_STYLE_FILL_AREA ( #4590 ) ;
#4628 = ORIENTED_EDGE ( 'NONE', *, *, #1282, .F. ) ;
#4629 = ADVANCED_FACE ( 'NONE', ( #3349 ), #7281, .F. ) ;
#4630 = CIRCLE ( 'NONE', #6606, 2.649999999999999467 ) ;
#4631 = AXIS2_PLACEMENT_3D ( 'NONE', #7475, #1790, #6177 ) ;
#4632 = CIRCLE ( 'NONE', #3440, 1.649999999999995248 ) ;
#4633 = PLANE ( 'NONE',  #3704 ) ;
#4634 = FACE_OUTER_BOUND ( 'NONE', #2952, .T. ) ;
#4635 = CARTESIAN_POINT ( 'NONE',  ( 2.000000000000000000, 1.880445160090761061E-16, -1.535500000000000087 ) ) ;
#4636 = EDGE_CURVE ( 'NONE', #6791, #5593, #3309, .T. ) ;
#4637 = AXIS2_PLACEMENT_3D ( 'NONE', #1431, #7813, #5335 ) ;
#4638 = CARTESIAN_POINT ( 'NONE',  ( -29.99999999999999289, 30.00000000000000711, 10.00000000000000000 ) ) ;
#4639 = AXIS2_PLACEMENT_3D ( 'NONE', #690, #143, #97 ) ;
#4640 = DIRECTION ( 'NONE',  ( -0.000000000000000000, 1.000000000000000000, -0.000000000000000000 ) ) ;
#4641 = ORIENTED_EDGE ( 'NONE', *, *, #3147, .F. ) ;
#4642 = DIRECTION ( 'NONE',  ( 0.000000000000000000, 0.000000000000000000, 1.000000000000000000 ) ) ;
#4643 = AXIS2_PLACEMENT_3D ( 'NONE', #5754, #45, #2597 ) ;
#4644 = CARTESIAN_POINT ( 'NONE',  ( -1.318516776095820964, -3.857556137907092175, -2.699999999999984190 ) ) ;
#4645 = DIRECTION ( 'NONE',  ( 0.000000000000000000, 0.000000000000000000, 1.000000000000000000 ) ) ;
#4646 = CARTESIAN_POINT ( 'NONE',  ( -54.99999999999990052, 10.00000000000000000, 17.64999999999876579 ) ) ;
#4647 = CARTESIAN_POINT ( 'NONE',  ( 55.00000000000000000, 10.00000000000000000, 17.64999999999999858 ) ) ;
#4648 = EDGE_LOOP ( 'NONE', ( #5486, #3335, #7759 ) ) ;
#4649 = AXIS2_PLACEMENT_3D ( 'NONE', #6202, #1056, #3733 ) ;
#4650 = DIRECTION ( 'NONE',  ( -1.000000000000000000, -0.000000000000000000, -0.000000000000000000 ) ) ;
#4651 = PRODUCT_DEFINITION_CONTEXT ( 'detailed design', #7191, 'design' ) ;
#4652 = EDGE_LOOP ( 'NONE', ( #4275, #2068 ) ) ;
#4653 =( REPRESENTATION_RELATIONSHIP ('NONE','NONE', #3916, #2475 ) REPRESENTATION_RELATIONSHIP_WITH_TRANSFORMATION ( #196 )SHAPE_REPRESENTATION_RELATIONSHIP( ) );
#4654 = ORIENTED_EDGE ( 'NONE', *, *, #3204, .F. ) ;
#4655 = AXIS2_PLACEMENT_3D ( 'NONE', #3637, #4975, #3099 ) ;
#4656 = LINE ( 'NONE', #2704, #2368 ) ;
#4657 = PLANE ( 'NONE',  #232 ) ;
#4658 = LINE ( 'NONE', #2788, #7137 ) ;
#4659 = PRODUCT_CONTEXT ( 'NONE', #5346, 'mechanical' ) ;
#4660 = EDGE_CURVE ( 'NONE', #1575, #3495, #5912, .T. ) ;
#4661 = ADVANCED_FACE ( 'NONE', ( #6497 ), #4633, .F. ) ;
#4662 = VERTEX_POINT ( 'NONE', #3980 ) ;
#4663 = VERTEX_POINT ( 'NONE', #2138 ) ;
#4664 = ORIENTED_EDGE ( 'NONE', *, *, #3552, .F. ) ;
#4665 = DIRECTION ( 'NONE',  ( 0.000000000000000000, -0.000000000000000000, -1.000000000000000000 ) ) ;
#4666 = CARTESIAN_POINT ( 'NONE',  ( 3.504480373706772234, -6.063947902487814012, 8.008485521361658144 ) ) ;
#4667 = CARTESIAN_POINT ( 'NONE',  ( -4.000000000000000000, 0.000000000000000000, 0.000000000000000000 ) ) ;
#4668 =( LENGTH_UNIT ( ) NAMED_UNIT ( * ) SI_UNIT ( .MILLI., .METRE. ) );
#4669 = ORIENTED_EDGE ( 'NONE', *, *, #3723, .T. ) ;
#4670 = CARTESIAN_POINT ( 'NONE',  ( -49.99999999999999289, 85.00000000000005684, 2.400000000000013234 ) ) ;
#4671 = VECTOR ( 'NONE', #6639, 1000.000000000000000 ) ;
#4672 = CARTESIAN_POINT ( 'NONE',  ( 1.257674520083185143E-14, 4.618802153517020948, -0.3572655899081733644 ) ) ;
#4673 = ADVANCED_FACE ( 'NONE', ( #3381 ), #771, .T. ) ;
#4674 = DIRECTION ( 'NONE',  ( -1.000000000000000000, 0.000000000000000000, 0.000000000000000000 ) ) ;
#4675 =( NAMED_UNIT ( * ) PLANE_ANGLE_UNIT ( ) SI_UNIT ( $, .RADIAN. ) );
#4676 = FACE_BOUND ( 'NONE', #1695, .T. ) ;
#4677 = CARTESIAN_POINT ( 'NONE',  ( 6.821338123897841221, 1.588166687390477616, 8.032256283446461254 ) ) ;
#4678 = ORIENTED_EDGE ( 'NONE', *, *, #6865, .T. ) ;
#4679 = CARTESIAN_POINT ( 'NONE',  ( -52.00000000000006395, 7.999999999999996447, 11.99999999999998934 ) ) ;
#4680 = CARTESIAN_POINT ( 'NONE',  ( 2.500000000000002220, 0.000000000000000000, 0.000000000000000000 ) ) ;
#4681 = CYLINDRICAL_SURFACE ( 'NONE', #1421, 7.000000000000000000 ) ;
#4682 = EDGE_CURVE ( 'NONE', #5522, #1297, #6749, .T. ) ;
#4683 = CARTESIAN_POINT ( 'NONE',  ( 52.00000000000000000, -8.000000000000003553, 19.99999999999998934 ) ) ;
#4684 = CARTESIAN_POINT ( 'NONE',  ( 29.99999999999997868, 30.00000000000001421, 4.599999999999997868 ) ) ;
#4685 = DIRECTION ( 'NONE',  ( 0.000000000000000000, 0.000000000000000000, 1.000000000000000000 ) ) ;
#4686 = PRODUCT_DEFINITION_FORMATION_WITH_SPECIFIED_SOURCE ( 'ANY', '', #1876, .NOT_KNOWN. ) ;
#4687 = DIRECTION ( 'NONE',  ( -1.000000000000000000, 0.000000000000000000, 1.412205397084726379E-17 ) ) ;
#4688 = VERTEX_POINT ( 'NONE', #295 ) ;
#4689 = LINE ( 'NONE', #5322, #4470 ) ;
#4690 = EDGE_LOOP ( 'NONE', ( #2327, #7439, #4011, #4736 ) ) ;
#4691 = ORIENTED_EDGE ( 'NONE', *, *, #60, .T. ) ;
#4692 = PRESENTATION_LAYER_ASSIGNMENT (  '', '', ( #5233 ) ) ;
#4693 = DIRECTION ( 'NONE',  ( 0.000000000000000000, 0.4999999999999990008, -0.8660254037844391517 ) ) ;
#4694 = FACE_OUTER_BOUND ( 'NONE', #1632, .T. ) ;
#4695 = EDGE_CURVE ( 'NONE', #2202, #6632, #4129, .T. ) ;
#4696 = DIRECTION ( 'NONE',  ( 0.000000000000000000, 1.000000000000000000, -1.224646799147353207E-16 ) ) ;
#4697 = CARTESIAN_POINT ( 'NONE',  ( -2.999999999999998668, 35.09008114612887397, 4.000000000000000000 ) ) ;
#4698 = ORIENTED_EDGE ( 'NONE', *, *, #7483, .F. ) ;
#4699 = ORIENTED_EDGE ( 'NONE', *, *, #3242, .T. ) ;
#4700 = EDGE_LOOP ( 'NONE', ( #3878, #6221, #1244, #782, #4495, #6047 ) ) ;
#4701 = CIRCLE ( 'NONE', #450, 2.500000000000000444 ) ;
#4702 = EDGE_CURVE ( 'NONE', #6468, #3614, #3708, .T. ) ;
#4703 = DIRECTION ( 'NONE',  ( 1.000000000000000000, 0.000000000000000000, 0.000000000000000000 ) ) ;
#4704 = CARTESIAN_POINT ( 'NONE',  ( 6.379742460914609836, -2.889908336535204292, 8.028210883294187639 ) ) ;
#4705 = DIRECTION ( 'NONE',  ( -1.000000000000000000, 0.000000000000000000, 0.000000000000000000 ) ) ;
#4706 = CARTESIAN_POINT ( 'NONE',  ( -2.500000000000000444, 3.061616997868384127E-16, 3.469446951953614189E-15 ) ) ;
#4707 = DIRECTION ( 'NONE',  ( -0.000000000000000000, -0.000000000000000000, -1.000000000000000000 ) ) ;
#4708 = DIRECTION ( 'NONE',  ( 0.000000000000000000, 0.000000000000000000, -1.000000000000000000 ) ) ;
#4709 = DIRECTION ( 'NONE',  ( 0.000000000000000000, 0.000000000000000000, 1.000000000000000000 ) ) ;
#4710 = DIRECTION ( 'NONE',  ( 0.000000000000000000, 0.000000000000000000, 1.000000000000000000 ) ) ;
#4711 = PRODUCT_RELATED_PRODUCT_CATEGORY ( 'part', '', ( #5068 ) ) ;
#4712 = ORIENTED_EDGE ( 'NONE', *, *, #6798, .T. ) ;
#4713 = EDGE_CURVE ( 'NONE', #5731, #3952, #1514, .T. ) ;
#4714 = VERTEX_POINT ( 'NONE', #4051 ) ;
#4715 = ADVANCED_FACE ( 'NONE', ( #6564 ), #3423, .F. ) ;
#4716 = CARTESIAN_POINT ( 'NONE',  ( 1.300000000000000044, -0.7390083445627200209, 1.280000000000001137 ) ) ;
#4717 = DIRECTION ( 'NONE',  ( 0.000000000000000000, 1.000000000000000000, -0.000000000000000000 ) ) ;
#4718 = DIRECTION ( 'NONE',  ( -0.000000000000000000, -0.000000000000000000, -1.000000000000000000 ) ) ;
#4719 = CARTESIAN_POINT ( 'NONE',  ( 4.199999999999995737, 0.000000000000000000, -2.200000000000001066 ) ) ;
#4720 = LINE ( 'NONE', #4848, #2380 ) ;
#4721 = CARTESIAN_POINT ( 'NONE',  ( -49.95346277782373079, 82.84241399044240950, -1.062802698623567466 ) ) ;
#4722 = DIRECTION ( 'NONE',  ( 0.000000000000000000, 1.000000000000000000, -0.000000000000000000 ) ) ;
#4723 = ORIENTED_EDGE ( 'NONE', *, *, #167, .F. ) ;
#4724 = DIRECTION ( 'NONE',  ( 0.000000000000000000, 0.000000000000000000, 1.000000000000000000 ) ) ;
#4725 = VECTOR ( 'NONE', #6547, 1000.000000000000227 ) ;
#4726 = ORIENTED_EDGE ( 'NONE', *, *, #1598, .F. ) ;
#4727 = ORIENTED_EDGE ( 'NONE', *, *, #6571, .F. ) ;
#4728 = CARTESIAN_POINT ( 'NONE',  ( -7.502679033599690683E-14, -4.618802153517020059, -2.342734410091827701 ) ) ;
#4729 = LINE ( 'NONE', #4817, #7014 ) ;
#4730 = CARTESIAN_POINT ( 'NONE',  ( 1.274374112546295138E-14, 85.00000000000017053, 2.000000000000043521 ) ) ;
#4731 = CARTESIAN_POINT ( 'NONE',  ( -4.000000000000000000, 2.309401076758496263, -0.3572655899081631503 ) ) ;
#4732 = LINE ( 'NONE', #950, #3175 ) ;
#4733 = ADVANCED_FACE ( 'NONE', ( #8023 ), #7325, .F. ) ;
#4734 = ORIENTED_EDGE ( 'NONE', *, *, #4034, .T. ) ;
#4735 = EDGE_CURVE ( 'NONE', #1969, #244, #6364, .T. ) ;
#4736 = ORIENTED_EDGE ( 'NONE', *, *, #5934, .T. ) ;
#4737 = EDGE_LOOP ( 'NONE', ( #519, #3797, #6690, #5629 ) ) ;
#4738 = DIRECTION ( 'NONE',  ( 0.000000000000000000, -0.000000000000000000, -1.000000000000000000 ) ) ;
#4739 = CARTESIAN_POINT ( 'NONE',  ( 0.000000000000000000, 0.000000000000000000, 3.299999999999999822 ) ) ;
#4740 = CONICAL_SURFACE ( 'NONE', #5546, 4.000000000000000000, 1.047197551196595855 ) ;
#4741 =( NAMED_UNIT ( * ) SI_UNIT ( $, .STERADIAN. ) SOLID_ANGLE_UNIT ( ) );
#4742 = CIRCLE ( 'NONE', #5935, 2.649999999999999467 ) ;
#4743 = FILL_AREA_STYLE_COLOUR ( '', #1060 ) ;
#4744 = CIRCLE ( 'NONE', #1165, 10.00000000000000000 ) ;
#4745 = VECTOR ( 'NONE', #1690, 1000.000000000000000 ) ;
#4746 = VECTOR ( 'NONE', #1884, 1000.000000000000000 ) ;
#4747 = LINE ( 'NONE', #2803, #1325 ) ;
#4748 = CARTESIAN_POINT ( 'NONE',  ( 2.500000000000002220, 1.178949249685212086, -2.042000000000002036 ) ) ;
#4749 = VECTOR ( 'NONE', #6374, 1000.000000000000000 ) ;
#4750 = DIRECTION ( 'NONE',  ( -0.000000000000000000, -0.000000000000000000, -1.000000000000000000 ) ) ;
#4751 = EDGE_CURVE ( 'NONE', #590, #708, #4169, .T. ) ;
#4752 = CIRCLE ( 'NONE', #1316, 4.999999999999993783 ) ;
#4753 = LINE ( 'NONE', #879, #5483 ) ;
#4754 = AXIS2_PLACEMENT_3D ( 'NONE', #142, #95, #2647 ) ;
#4755 = AXIS2_PLACEMENT_3D ( 'NONE', #4984, #7505, #1993 ) ;
#4756 = EDGE_CURVE ( 'NONE', #5567, #2900, #4233, .T. ) ;
#4757 = VECTOR ( 'NONE', #1829, 1000.000000000000000 ) ;
#4758 = EDGE_LOOP ( 'NONE', ( #1473, #4041, #7220, #7303, #1879, #7852 ) ) ;
#4759 = ORIENTED_EDGE ( 'NONE', *, *, #1541, .T. ) ;
#4760 = CARTESIAN_POINT ( 'NONE',  ( -31.74999999999995737, 1.836970198721030181E-16, -1.500000000000000222 ) ) ;
#4761 = DIRECTION ( 'NONE',  ( -0.8660254037844347108, 0.5000000000000066613, 0.000000000000000000 ) ) ;
#4762 = CARTESIAN_POINT ( 'NONE',  ( 55.00000000000000000, 8.000000000000000000, -2.849999999999991651 ) ) ;
#4763 = CIRCLE ( 'NONE', #1186, 2.649999999999995914 ) ;
#4764 = CARTESIAN_POINT ( 'NONE',  ( 60.00000000000014211, 10.00000000000000000, 10.50000000000006395 ) ) ;
#4765 = CARTESIAN_POINT ( 'NONE',  ( 52.00000000000000711, -8.000000000000000000, -8.000000000000000000 ) ) ;
#4766 = PLANE ( 'NONE',  #6496 ) ;
#4767 = CARTESIAN_POINT ( 'NONE',  ( 55.00000000000000000, 10.00000000000000000, 13.35000000000000497 ) ) ;
#4768 = VERTEX_POINT ( 'NONE', #1643 ) ;
#4769 = CIRCLE ( 'NONE', #6614, 2.149999999999999023 ) ;
#4770 = DIRECTION ( 'NONE',  ( -0.8660254037844372643, -0.5000000000000023315, 0.000000000000000000 ) ) ;
#4771 = VECTOR ( 'NONE', #6024, 1000.000000000000000 ) ;
#4772 = ORIENTED_EDGE ( 'NONE', *, *, #6672, .T. ) ;
#4773 = AXIS2_PLACEMENT_3D ( 'NONE', #7894, #874, #7282 ) ;
#4774 = EDGE_LOOP ( 'NONE', ( #6646, #42, #5808, #2001, #57 ) ) ;
#4775 = AXIS2_PLACEMENT_3D ( 'NONE', #6965, #1780, #4310 ) ;
#4776 = CARTESIAN_POINT ( 'NONE',  ( -3.000000000000000888, 45.09008114612887397, 4.000000000000000000 ) ) ;
#4777 = LINE ( 'NONE', #7309, #5425 ) ;
#4778 = DIRECTION ( 'NONE',  ( 0.000000000000000000, -0.4999999999999993339, 0.8660254037844389297 ) ) ;
#4779 = DIRECTION ( 'NONE',  ( -1.000000000000000000, 0.000000000000000000, 0.000000000000000000 ) ) ;
#4780 = ADVANCED_FACE ( 'NONE', ( #3545 ), #112, .F. ) ;
#4781 = VECTOR ( 'NONE', #5464, 1000.000000000000227 ) ;
#4782 = FACE_OUTER_BOUND ( 'NONE', #5222, .T. ) ;
#4783 = APPLICATION_PROTOCOL_DEFINITION ( 'draft international standard', 'automotive_design', 1998, #509 ) ;
#4785 = EDGE_CURVE ( 'NONE', #5103, #6416, #6825, .T. ) ;
#4784 = AXIS2_PLACEMENT_3D ( 'NONE', #4544, #7069, #6442 ) ;
#4786 = EDGE_LOOP ( 'NONE', ( #6813, #1558, #5058 ) ) ;
#4787 = ORIENTED_EDGE ( 'NONE', *, *, #3972, .F. ) ;
#4788 = ORIENTED_EDGE ( 'NONE', *, *, #5024, .F. ) ;
#4789 = ADVANCED_FACE ( 'NONE', ( #7406, #4337, #4879 ), #7496, .T. ) ;
#4790 = FACE_OUTER_BOUND ( 'NONE', #994, .T. ) ;
#4791 = CARTESIAN_POINT ( 'NONE',  ( 6.954242511297643148, -0.9206211859927554420, 8.033521398158129045 ) ) ;
#4792 = DIRECTION ( 'NONE',  ( 0.000000000000000000, 1.000000000000000000, -0.000000000000000000 ) ) ;
#4793 = EDGE_CURVE ( 'NONE', #166, #3060, #3979, .T. ) ;
#4794 = EDGE_LOOP ( 'NONE', ( #8176, #4305, #943, #5869, #1381, #2395, #2632 ) ) ;
#4795 = FACE_OUTER_BOUND ( 'NONE', #7403, .T. ) ;
#4796 = B_SPLINE_CURVE_WITH_KNOTS ( 'NONE', 3,
 ( #4282, #4239, #5493, #6807, #1116, #5575, #4116, #8004, #6768, #3659, #7261, #2287, #1581, #6016, #6682, #4821, #7349, #2863, #7918, #7311, #1625, #4155 ),
 .UNSPECIFIED., .F., .F.,
 ( 4, 2, 2, 2, 2, 2, 2, 2, 2, 2, 4 ),
 ( 0.03283134218946166805, 0.03419813915831548812, 0.03488153764274239815, 0.03556493612716930819, 0.03693173309602312826, 0.03829853006487694833, 0.03966532703373076840, 0.04034872551815767844, 0.04103212400258458847, 0.04239892097143841548, 0.04376571794029223555 ),
 .UNSPECIFIED. ) ;
#4797 = LINE ( 'NONE', #1679, #118 ) ;
#4798 = DIRECTION ( 'NONE',  ( 0.000000000000000000, -1.000000000000000000, 0.000000000000000000 ) ) ;
#4799 = DIRECTION ( 'NONE',  ( -1.000000000000000000, -0.000000000000000000, -0.000000000000000000 ) ) ;
#4800 = DIRECTION ( 'NONE',  ( 1.000000000000000000, 0.000000000000000000, 0.000000000000000000 ) ) ;
#4801 = VECTOR ( 'NONE', #6722, 1000.000000000000000 ) ;
#4802 = EDGE_LOOP ( 'NONE', ( #453, #2476, #6388, #6100 ) ) ;
#4803 = EDGE_LOOP ( 'NONE', ( #2235, #1331, #3717, #5204, #2512, #7427, #2602 ) ) ;
#4804 = CARTESIAN_POINT ( 'NONE',  ( -29.99999999999999289, 30.00000000000000711, 10.00000000000000000 ) ) ;
#4805 = CARTESIAN_POINT ( 'NONE',  ( 29.55500000000002458, 0.000000000000000000, -6.938893903907228378E-15 ) ) ;
#4806 = CARTESIAN_POINT ( 'NONE',  ( 2.500000000000002220, 2.357898499370434386, -3.469446951953614189E-15 ) ) ;
#4807 = CARTESIAN_POINT ( 'NONE',  ( 4.199999999999995737, 0.000000000000000000, 0.000000000000000000 ) ) ;
#4808 = FACE_OUTER_BOUND ( 'NONE', #1430, .T. ) ;
#4809 = DIRECTION ( 'NONE',  ( -0.000000000000000000, -0.000000000000000000, 1.000000000000000000 ) ) ;
#4810 = AXIS2_PLACEMENT_3D ( 'NONE', #4175, #7169, #2807 ) ;
#4811 = CARTESIAN_POINT ( 'NONE',  ( -31.74999999999994316, 0.000000000000000000, 0.000000000000000000 ) ) ;
#4812 = ORIENTED_EDGE ( 'NONE', *, *, #6407, .F. ) ;
#4813 = LINE ( 'NONE', #3485, #2997 ) ;
#4814 = VERTEX_POINT ( 'NONE', #4260 ) ;
#4815 = VERTEX_POINT ( 'NONE', #1134 ) ;
#4816 = CARTESIAN_POINT ( 'NONE',  ( 2.500000000000002220, -3.469446951953614189E-15, -2.041999999999998483 ) ) ;
#4817 = CARTESIAN_POINT ( 'NONE',  ( 2.999999999999999112, 45.09008114612887397, 4.000000000000000000 ) ) ;
#4818 = ADVANCED_FACE ( 'NONE', ( #6076 ), #6786, .F. ) ;
#4819 = CARTESIAN_POINT ( 'NONE',  ( -39.99999999999999289, 40.00000000000000711, 0.000000000000000000 ) ) ;
#4820 = B_SPLINE_CURVE_WITH_KNOTS ( 'NONE', 3,
 ( #2265, #426, #8070, #382, #4300, #6828, #7327, #1645, #4174, #8154, #2641, #2028, #5190, #7709, #2473, #1399, #5070, #7044, #2521, #4471, #1986, #1313, #8194 ),
 .UNSPECIFIED., .F., .F.,
 ( 4, 2, 2, 2, 2, 2, 2, 2, 1, 2, 2, 4 ),
 ( 6.815276097578277091E-20, 0.001368142784595155264, 0.002052214176892732354, 0.002736285569190309661, 0.004104428353785464709, 0.005472571138380617588, 0.006840713922975770467, 0.007524785315273349075, 0.008208856707570925948, 0.008892928099868503689, 0.009576999492166081429, 0.01094514227676123691 ),
 .UNSPECIFIED. ) ;
#4821 = CARTESIAN_POINT ( 'NONE',  ( -6.279904204137568335, 3.100863108398094425, 8.027331884377945315 ) ) ;
#4822 = FILL_AREA_STYLE_COLOUR ( '', #2889 ) ;
#4823 = MECHANICAL_DESIGN_GEOMETRIC_PRESENTATION_REPRESENTATION (  '', ( #1106 ), #6284 ) ;
#4824 = ORIENTED_EDGE ( 'NONE', *, *, #7943, .F. ) ;
#4825 = ADVANCED_FACE ( 'NONE', ( #5547 ), #379, .F. ) ;
#4826 = ORIENTED_EDGE ( 'NONE', *, *, #7470, .F. ) ;
#4827 = ORIENTED_EDGE ( 'NONE', *, *, #667, .F. ) ;
#4828 = EDGE_CURVE ( 'NONE', #3881, #4888, #6743, .T. ) ;
#4829 = EDGE_CURVE ( 'NONE', #3851, #1575, #7361, .T. ) ;
#4830 = DIRECTION ( 'NONE',  ( 0.000000000000000000, -1.000000000000000000, 1.222984857324291014E-15 ) ) ;
#4831 = CARTESIAN_POINT ( 'NONE',  ( 58.00000000000000000, 8.000000000000000000, -8.000000000000000000 ) ) ;
#4832 = CARTESIAN_POINT ( 'NONE',  ( 0.000000000000000000, 0.000000000000000000, 4.000000000000000000 ) ) ;
#4833 =( GEOMETRIC_REPRESENTATION_CONTEXT ( 3 ) GLOBAL_UNCERTAINTY_ASSIGNED_CONTEXT ( ( #2732 ) ) GLOBAL_UNIT_ASSIGNED_CONTEXT ( ( #7276, #6527, #4923 ) ) REPRESENTATION_CONTEXT ( 'NONE', 'WORKASPACE' ) );
#4834 = EDGE_LOOP ( 'NONE', ( #7316, #1275, #746, #3963 ) ) ;
#4835 = CARTESIAN_POINT ( 'NONE',  ( 4.000000000000004441, 0.7862748000878159171, -0.03447227762756881198 ) ) ;
#4836 = EDGE_LOOP ( 'NONE', ( #4078, #8179, #2054, #5631 ) ) ;
#4837 = CARTESIAN_POINT ( 'NONE',  ( 41.99060366484418694, 85.91597045152531109, 2.230540027468066899 ) ) ;
#4838 = DIRECTION ( 'NONE',  ( 0.000000000000000000, 0.000000000000000000, -1.000000000000000000 ) ) ;
#4839 = PRODUCT ( 'socket head cap screw_iso_ISO 4762 M4 x 20 - 20N', 'socket head cap screw_iso_ISO 4762 M4 x 20 - 20N', '', ( #7225 ) ) ;
#4840 = CARTESIAN_POINT ( 'NONE',  ( 2.500000000000002220, 2.500728763858895382E-16, -2.041999999999999815 ) ) ;
#4841 = FACE_BOUND ( 'NONE', #315, .T. ) ;
#4842 = EDGE_CURVE ( 'NONE', #3182, #4877, #4797, .T. ) ;
#4843 = ORIENTED_EDGE ( 'NONE', *, *, #5499, .T. ) ;
#4844 = ORIENTED_EDGE ( 'NONE', *, *, #3459, .F. ) ;
#4845 = LINE ( 'NONE', #4220, #491 ) ;
#4846 = FACE_OUTER_BOUND ( 'NONE', #4786, .T. ) ;
#4847 = DIRECTION ( 'NONE',  ( 1.000000000000000000, 0.000000000000000000, 0.000000000000000000 ) ) ;
#4848 = CARTESIAN_POINT ( 'NONE',  ( 58.00000000000000000, -8.000000000000000000, -8.000000000000000000 ) ) ;
#4849 = DIRECTION ( 'NONE',  ( -1.000000000000000000, -0.000000000000000000, -0.000000000000000000 ) ) ;
#4850 = ADVANCED_FACE ( 'NONE', ( #3095 ), #4208, .F. ) ;
#4851 = CARTESIAN_POINT ( 'NONE',  ( 34.99999999999997868, 30.00000000000001421, 4.599999999999997868 ) ) ;
#4852 = VERTEX_POINT ( 'NONE', #2604 ) ;
#4853 = CARTESIAN_POINT ( 'NONE',  ( -54.99999999999990052, 10.00000000000000000, 15.49999999999877254 ) ) ;
#4854 = EDGE_LOOP ( 'NONE', ( #1670, #4826, #541, #8199, #4930 ) ) ;
#4855 = VERTEX_POINT ( 'NONE', #87 ) ;
#4856 = PLANE ( 'NONE',  #6219 ) ;
#4857 = CYLINDRICAL_SURFACE ( 'NONE', #7412, 2.149999999999995470 ) ;
#4858 = CARTESIAN_POINT ( 'NONE',  ( 9.020562075079396891E-14, 10.00000000000000000, 8.000000000000007105 ) ) ;
#4859 = DIRECTION ( 'NONE',  ( 0.000000000000000000, -1.000000000000000000, 1.467581828789149729E-15 ) ) ;
#4860 = VECTOR ( 'NONE', #4107, 1000.000000000000000 ) ;
#4861 = CONTEXT_DEPENDENT_SHAPE_REPRESENTATION ( #7587, #2978 ) ;
#4862 = EDGE_CURVE ( 'NONE', #1812, #4465, #3318, .T. ) ;
#4863 = EDGE_LOOP ( 'NONE', ( #83, #5905, #6021, #6396, #5933, #647 ) ) ;
#4864 = EDGE_CURVE ( 'NONE', #7441, #550, #779, .T. ) ;
#4865 = VECTOR ( 'NONE', #5478, 1000.000000000000114 ) ;
#4866 = ORIENTED_EDGE ( 'NONE', *, *, #325, .F. ) ;
#4867 = AXIS2_PLACEMENT_3D ( 'NONE', #5690, #1069, #6840 ) ;
#4868 = ORIENTED_EDGE ( 'NONE', *, *, #6337, .F. ) ;
#4869 = ADVANCED_BREP_SHAPE_REPRESENTATION ( '', ( #6918, #1587 ), #2170 ) ;
#4870 = LINE ( 'NONE', #8105, #6616 ) ;
#4871 = FACE_OUTER_BOUND ( 'NONE', #3624, .T. ) ;
#4872 = CARTESIAN_POINT ( 'NONE',  ( 0.000000000000000000, -0.8865213383406690406, 1.535500000000000975 ) ) ;
#4873 = UNCERTAINTY_MEASURE_WITH_UNIT (LENGTH_MEASURE( 1.000000000000000082E-05 ), #3604, 'distance_accuracy_value', 'NONE');
#4874 = VERTEX_POINT ( 'NONE', #18 ) ;
#4875 = CARTESIAN_POINT ( 'NONE',  ( 4.000000000000003553, 2.309401076758524685, -0.3572655899081733644 ) ) ;
#4876 = ORIENTED_EDGE ( 'NONE', *, *, #7515, .T. ) ;
#4877 = VERTEX_POINT ( 'NONE', #6994 ) ;
#4878 = CONICAL_SURFACE ( 'NONE', #4082, 4.000000000000000000, 1.047197551196595855 ) ;
#4879 = FACE_OUTER_BOUND ( 'NONE', #2775, .T. ) ;
#4880 = PLANE ( 'NONE',  #4380 ) ;
#4881 = AXIS2_PLACEMENT_3D ( 'NONE', #4057, #4100, #7832 ) ;
#4882 = EDGE_CURVE ( 'NONE', #2560, #1740, #7557, .T. ) ;
#4883 = FACE_OUTER_BOUND ( 'NONE', #8059, .T. ) ;
#4884 = ADVANCED_FACE ( 'NONE', ( #749, #5722, #1979, #7589, #595, #6381 ), #7660, .F. ) ;
#4885 = CARTESIAN_POINT ( 'NONE',  ( 2.250597875665110603, 6.632329153766082008, 8.003477766920562786 ) ) ;
#4886 = AXIS2_PLACEMENT_3D ( 'NONE', #522, #566, #3108 ) ;
#4887 = VERTEX_POINT ( 'NONE', #2564 ) ;
#4888 = VERTEX_POINT ( 'NONE', #7040 ) ;
#4889 = EDGE_CURVE ( 'NONE', #972, #3630, #6089, .T. ) ;
#4890 = SURFACE_STYLE_USAGE ( .BOTH. , #2398 ) ;
#4891 = DIRECTION ( 'NONE',  ( 0.000000000000000000, 0.000000000000000000, 1.000000000000000000 ) ) ;
#4892 = DIRECTION ( 'NONE',  ( 0.000000000000000000, 1.000000000000000000, -1.467581828789149532E-15 ) ) ;
#4893 = DIRECTION ( 'NONE',  ( -0.000000000000000000, -0.000000000000000000, -1.000000000000000000 ) ) ;
#4894 = VECTOR ( 'NONE', #6587, 1000.000000000000000 ) ;
#4895 = AXIS2_PLACEMENT_3D ( 'NONE', #2543, #3118, #5086 ) ;
#4896 = VECTOR ( 'NONE', #4038, 1000.000000000000114 ) ;
#4897 = DIRECTION ( 'NONE',  ( 1.000000000000000000, 0.000000000000000000, 0.000000000000000000 ) ) ;
#4898 = CARTESIAN_POINT ( 'NONE',  ( 1.300000000000000044, 0.7390083445627193548, -1.280000000000000693 ) ) ;
#4899 = ORIENTED_EDGE ( 'NONE', *, *, #7860, .F. ) ;
#4900 = VERTEX_POINT ( 'NONE', #5107 ) ;
#4901 = COLOUR_RGB ( '', 0.09019608, 0.27058824, 0.51372549) ;
#4902 = AXIS2_PLACEMENT_3D ( 'NONE', #6530, #7123, #4087 ) ;
#4903 = DIRECTION ( 'NONE',  ( -1.000000000000000000, -0.000000000000000000, -0.000000000000000000 ) ) ;
#4904 = CIRCLE ( 'NONE', #4000, 2.500000000000000888 ) ;
#4905 = DIRECTION ( 'NONE',  ( 0.000000000000000000, 0.000000000000000000, 1.000000000000000000 ) ) ;
#4906 = DIRECTION ( 'NONE',  ( 0.000000000000000000, -0.4999999999999992228, 0.8660254037844390407 ) ) ;
#4907 = DIRECTION ( 'NONE',  ( 1.000000000000000000, 0.000000000000000000, 0.000000000000000000 ) ) ;
#4908 = CARTESIAN_POINT ( 'NONE',  ( 60.00000000000000711, -10.00000000000000000, 0.000000000000000000 ) ) ;
#4909 = PLANE ( 'NONE',  #3299 ) ;
#4910 = AXIS2_PLACEMENT_3D ( 'NONE', #1930, #5784, #707 ) ;
#4911 = ORIENTED_EDGE ( 'NONE', *, *, #6302, .T. ) ;
#4912 = VECTOR ( 'NONE', #2025, 1000.000000000000000 ) ;
#4913 = CIRCLE ( 'NONE', #8085, 2.055000000000000160 ) ;
#4914 = VECTOR ( 'NONE', #4685, 1000.000000000000000 ) ;
#4915 = ORIENTED_EDGE ( 'NONE', *, *, #485, .F. ) ;
#4916 = VERTEX_POINT ( 'NONE', #3300 ) ;
#4917 = ORIENTED_EDGE ( 'NONE', *, *, #1924, .F. ) ;
#4918 = PRODUCT_DEFINITION_SHAPE ( 'NONE', 'NONE',  #8215 ) ;
#4919 = DIRECTION ( 'NONE',  ( 0.000000000000000000, -0.000000000000000000, 1.000000000000000000 ) ) ;
#4920 = CARTESIAN_POINT ( 'NONE',  ( -52.00000000000006395, 7.999999999999996447, 19.99999999999998934 ) ) ;
#4921 = VECTOR ( 'NONE', #1893, 1000.000000000000000 ) ;
#4922 = DIRECTION ( 'NONE',  ( 0.000000000000000000, 0.000000000000000000, 1.000000000000000000 ) ) ;
#4923 =( NAMED_UNIT ( * ) SI_UNIT ( $, .STERADIAN. ) SOLID_ANGLE_UNIT ( ) );
#4924 = EDGE_CURVE ( 'NONE', #5583, #7658, #2516, .T. ) ;
#4925 = EDGE_CURVE ( 'NONE', #7076, #6632, #1309, .T. ) ;
#4926 = EDGE_LOOP ( 'NONE', ( #3794, #3568, #5584, #6751 ) ) ;
#4927 = DIRECTION ( 'NONE',  ( -1.000000000000000000, 0.000000000000000000, 0.000000000000000000 ) ) ;
#4928 = CIRCLE ( 'NONE', #2396, 50.00000000000002132 ) ;
#4929 = ORIENTED_EDGE ( 'NONE', *, *, #3669, .F. ) ;
#4930 = ORIENTED_EDGE ( 'NONE', *, *, #48, .T. ) ;
#4931 = AXIS2_PLACEMENT_3D ( 'NONE', #3785, #5119, #6427 ) ;
#4932 = DIRECTION ( 'NONE',  ( -1.000000000000000000, 0.000000000000000000, 0.000000000000000000 ) ) ;
#4933 = CARTESIAN_POINT ( 'NONE',  ( -41.93354940223068894, 82.63827966896762689, -0.4455622145786132249 ) ) ;
#4934 = DIRECTION ( 'NONE',  ( 0.000000000000000000, 0.000000000000000000, 1.000000000000000000 ) ) ;
#4935 = CARTESIAN_POINT ( 'NONE',  ( 3.999999999999989786, -2.309401076758547777, -2.342734410091827701 ) ) ;
#4936 = CARTESIAN_POINT ( 'NONE',  ( 1.300000000000000044, -1.314525273895014473E-15, -1.280000000000000027 ) ) ;
#4937 = EDGE_CURVE ( 'NONE', #2420, #5782, #6291, .T. ) ;
#4938 = ADVANCED_FACE ( 'NONE', ( #3892 ), #2636, .T. ) ;
#4939 = VERTEX_POINT ( 'NONE', #5064 ) ;
#4940 = VERTEX_POINT ( 'NONE', #5011 ) ;
#4941 =( NAMED_UNIT ( * ) SI_UNIT ( $, .STERADIAN. ) SOLID_ANGLE_UNIT ( ) );
#4942 = DIRECTION ( 'NONE',  ( 1.000000000000000000, 0.000000000000000000, 0.000000000000000000 ) ) ;
#4943 = DIRECTION ( 'NONE',  ( -0.000000000000000000, -0.000000000000000000, 1.000000000000000000 ) ) ;
#4944 = CARTESIAN_POINT ( 'NONE',  ( 2.000000000000000000, -0.8865213383406721492, -1.535499999999999199 ) ) ;
#4945 = DIRECTION ( 'NONE',  ( 1.000000000000000000, 0.000000000000000000, 0.000000000000000000 ) ) ;
#4946 = DIRECTION ( 'NONE',  ( 0.000000000000000000, 0.000000000000000000, 1.000000000000000000 ) ) ;
#4947 = CIRCLE ( 'NONE', #2948, 2.000000000000000888 ) ;
#4948 = VERTEX_POINT ( 'NONE', #7534 ) ;
#4949 = VERTEX_POINT ( 'NONE', #719 ) ;
#4950 = CARTESIAN_POINT ( 'NONE',  ( 2.000000000000000000, 0.000000000000000000, 0.000000000000000000 ) ) ;
#4951 = LINE ( 'NONE', #6890, #7806 ) ;
#4952 = DIRECTION ( 'NONE',  ( 1.000000000000000000, 0.000000000000000000, 0.000000000000000000 ) ) ;
#4953 = CARTESIAN_POINT ( 'NONE',  ( 3.999999999999997335, 2.694222958124178486E-16, 2.200000000000001066 ) ) ;
#4954 = VECTOR ( 'NONE', #929, 1000.000000000000000 ) ;
#4955 = DIRECTION ( 'NONE',  ( 1.000000000000000000, 0.000000000000000000, -2.065146995210483462E-17 ) ) ;
#4956 = CARTESIAN_POINT ( 'NONE',  ( -2.650000000000003020, 0.000000000000000000, 0.000000000000000000 ) ) ;
#4957 = ORIENTED_EDGE ( 'NONE', *, *, #7093, .T. ) ;
#4958 = ORIENTED_EDGE ( 'NONE', *, *, #7859, .F. ) ;
#4959 = ORIENTED_EDGE ( 'NONE', *, *, #5063, .T. ) ;
#4960 = EDGE_CURVE ( 'NONE', #5220, #6466, #1267, .T. ) ;
#4961 = ORIENTED_EDGE ( 'NONE', *, *, #1159, .T. ) ;
#4962 = DIRECTION ( 'NONE',  ( 1.412205397084880761E-17, 2.775557561562891967E-17, 1.000000000000000000 ) ) ;
#4963 = LINE ( 'NONE', #1672, #2918 ) ;
#4964 = FACE_OUTER_BOUND ( 'NONE', #6904, .T. ) ;
#4965 =( NAMED_UNIT ( * ) PLANE_ANGLE_UNIT ( ) SI_UNIT ( $, .RADIAN. ) );
#4966 =( GEOMETRIC_REPRESENTATION_CONTEXT ( 3 ) GLOBAL_UNCERTAINTY_ASSIGNED_CONTEXT ( ( #5540 ) ) GLOBAL_UNIT_ASSIGNED_CONTEXT ( ( #2304, #4675, #2759 ) ) REPRESENTATION_CONTEXT ( 'NONE', 'WORKASPACE' ) );
#4967 = ORIENTED_EDGE ( 'NONE', *, *, #6422, .T. ) ;
#4968 = DIRECTION ( 'NONE',  ( -0.5000000000000057732, -0.8660254037844353769, 0.000000000000000000 ) ) ;
#4969 = EDGE_LOOP ( 'NONE', ( #4326, #352, #2594 ) ) ;
#4970 = ORIENTED_EDGE ( 'NONE', *, *, #2136, .F. ) ;
#4971 = AXIS2_PLACEMENT_3D ( 'NONE', #2600, #5756, #81 ) ;
#4972 = DIRECTION ( 'NONE',  ( -1.000000000000000000, -0.000000000000000000, -0.000000000000000000 ) ) ;
#4973 = CARTESIAN_POINT ( 'NONE',  ( -30.00000000000000355, -29.99999999999999289, 10.00000000000000000 ) ) ;
#4974 =( NAMED_UNIT ( * ) PLANE_ANGLE_UNIT ( ) SI_UNIT ( $, .RADIAN. ) );
#4975 = DIRECTION ( 'NONE',  ( -1.000000000000000000, -0.000000000000000000, -0.000000000000000000 ) ) ;
#4976 = AXIS2_PLACEMENT_3D ( 'NONE', #5791, #4583, #1352 ) ;
#4977 = CARTESIAN_POINT ( 'NONE',  ( 40.00000000000000711, -39.99999999999999289, 10.00000000000000000 ) ) ;
#4978 = EDGE_CURVE ( 'NONE', #6902, #2202, #3811, .T. ) ;
#4979 = ORIENTED_EDGE ( 'NONE', *, *, #2119, .F. ) ;
#4980 = ORIENTED_EDGE ( 'NONE', *, *, #2458, .T. ) ;
#4981 = VECTOR ( 'NONE', #6622, 1000.000000000000114 ) ;
#4982 = CARTESIAN_POINT ( 'NONE',  ( 2.000000000000000000, 0.000000000000000000, 0.000000000000000000 ) ) ;
#4983 = FACE_BOUND ( 'NONE', #7567, .T. ) ;
#4984 = CARTESIAN_POINT ( 'NONE',  ( -3.469446951953613006E-15, 0.000000000000000000, 14.60000000000000142 ) ) ;
#4985 = PLANE ( 'NONE',  #130 ) ;
#4986 = PLANE ( 'NONE',  #3321 ) ;
#4987 = CARTESIAN_POINT ( 'NONE',  ( 4.199999999999995737, 0.000000000000000000, 0.000000000000000000 ) ) ;
#4988 = PRODUCT_DEFINITION_SHAPE ( 'NONE', 'NONE',  #8219 ) ;
#4989 = ORIENTED_EDGE ( 'NONE', *, *, #1212, .T. ) ;
#4990 = CARTESIAN_POINT ( 'NONE',  ( -2.999999999999998668, 35.09008114612887397, 0.000000000000000000 ) ) ;
#4991 = PLANE ( 'NONE',  #4754 ) ;
#4992 = CARTESIAN_POINT ( 'NONE',  ( 55.00000000000000000, 7.999999999999996447, 15.50000000000000355 ) ) ;
#4993 = DIRECTION ( 'NONE',  ( 0.000000000000000000, 0.000000000000000000, 1.000000000000000000 ) ) ;
#4994 = CARTESIAN_POINT ( 'NONE',  ( -0.6554360035617892155, 4.240386000424039459, -2.541324518471509641 ) ) ;
#4995 = DIRECTION ( 'NONE',  ( 0.000000000000000000, 0.000000000000000000, 1.000000000000000000 ) ) ;
#4996 = CONTEXT_DEPENDENT_SHAPE_REPRESENTATION ( #6287, #3731 ) ;
#4997 = VERTEX_POINT ( 'NONE', #1861 ) ;
#4998 = ORIENTED_EDGE ( 'NONE', *, *, #1784, .F. ) ;
#4999 = ORIENTED_EDGE ( 'NONE', *, *, #6818, .T. ) ;
#5000 = ORIENTED_EDGE ( 'NONE', *, *, #3134, .F. ) ;
#5001 = VECTOR ( 'NONE', #2921, 1000.000000000000000 ) ;
#5002 = CYLINDRICAL_SURFACE ( 'NONE', #7799, 721.2499999999977263 ) ;
#5004 = EDGE_CURVE ( 'NONE', #5123, #7060, #1332, .T. ) ;
#5003 = DIRECTION ( 'NONE',  ( 1.000000000000000000, 0.000000000000000000, 0.000000000000000000 ) ) ;
#5005 = DIRECTION ( 'NONE',  ( 1.000000000000000000, 0.000000000000000000, 0.000000000000000000 ) ) ;
#5006 = ORIENTED_EDGE ( 'NONE', *, *, #100, .T. ) ;
#5007 = CARTESIAN_POINT ( 'NONE',  ( 49.99423685432767428, 84.22705925652886094, 2.277573141052954053 ) ) ;
#5008 = AXIS2_PLACEMENT_3D ( 'NONE', #5851, #1445, #4444 ) ;
#5009 = ORIENTED_EDGE ( 'NONE', *, *, #5203, .F. ) ;
#5010 = ORIENTED_EDGE ( 'NONE', *, *, #4842, .T. ) ;
#5011 = CARTESIAN_POINT ( 'NONE',  ( 4.999999999999990230, 0.000000000000000000, 14.60000000000000142 ) ) ;
#5012 = CARTESIAN_POINT ( 'NONE',  ( 50.00000000000000000, 9.332579536216795825E-15, 54.99999999999997868 ) ) ;
#5013 = LINE ( 'NONE', #6252, #1837 ) ;
#5014 =( NAMED_UNIT ( * ) SI_UNIT ( $, .STERADIAN. ) SOLID_ANGLE_UNIT ( ) );
#5015 = CARTESIAN_POINT ( 'NONE',  ( 60.00000000000004263, 85.00000000000051159, -1.387778780781445676E-14 ) ) ;
#5016 = DIRECTION ( 'NONE',  ( 0.000000000000000000, 0.000000000000000000, -1.000000000000000000 ) ) ;
#5017 = ORIENTED_EDGE ( 'NONE', *, *, #354, .F. ) ;
#5018 = VERTEX_POINT ( 'NONE', #4388 ) ;
#5019 = DIRECTION ( 'NONE',  ( -0.000000000000000000, -0.000000000000000000, 1.000000000000000000 ) ) ;
#5020 = LINE ( 'NONE', #7504, #5696 ) ;
#5021 = FACE_OUTER_BOUND ( 'NONE', #7865, .T. ) ;
#5022 = ADVANCED_FACE ( 'NONE', ( #3139 ), #1943, .F. ) ;
#5023 = CARTESIAN_POINT ( 'NONE',  ( 4.000000000000003553, -2.309401076758539784, -2.700000000000000178 ) ) ;
#5024 = EDGE_CURVE ( 'NONE', #7730, #4218, #659, .T. ) ;
#5025 = B_SPLINE_CURVE_WITH_KNOTS ( 'NONE', 3,
 ( #5576, #428, #6939, #3121, #1834, #3793, #2493, #6275, #1251, #6314, #6848, #5658, #578, #8172, #3164, #3700, #1756, #3213, #5699, #6359, #4364, #6894, #2548, #3079, #666, #6808, #5038, #7566, #1926, #5745 ),
 .UNSPECIFIED., .F., .F.,
 ( 4, 2, 2, 2, 2, 2, 2, 2, 2, 2, 2, 2, 2, 2, 4 ),
 ( 0.007504573511820881310, 0.007973502549960435198, 0.008442431588099987352, 0.009380289664379093395, 0.009849218702518631671, 0.01031814774065816995, 0.01078707677879770822, 0.01125600581693724650, 0.01172493485507678478, 0.01219386389321632305, 0.01266279293135586133, 0.01313172196949539960, 0.01360065100763493788, 0.01406958004577447789, 0.01500743812205355444 ),
 .UNSPECIFIED. ) ;
#5026 = AXIS2_PLACEMENT_3D ( 'NONE', #3856, #5724, #3141 ) ;
#5027 = CARTESIAN_POINT ( 'NONE',  ( 2.500000000000002220, -1.178949249685215417, 2.042000000000002036 ) ) ;
#5028 = EDGE_CURVE ( 'NONE', #4948, #6759, #2834, .T. ) ;
#5029 = AXIS2_PLACEMENT_3D ( 'NONE', #6624, #7244, #6087 ) ;
#5030 = DIRECTION ( 'NONE',  ( -1.000000000000000000, -0.000000000000000000, -0.000000000000000000 ) ) ;
#5031 = ORIENTED_EDGE ( 'NONE', *, *, #6993, .F. ) ;
#5032 = CARTESIAN_POINT ( 'NONE',  ( 0.000000000000000000, 0.000000000000000000, 10.00000000000000000 ) ) ;
#5033 = DIRECTION ( 'NONE',  ( 1.000000000000000000, 0.000000000000000000, -0.000000000000000000 ) ) ;
#5034 = DIRECTION ( 'NONE',  ( 1.000000000000000000, 0.000000000000000000, 0.000000000000000000 ) ) ;
#5035 = CARTESIAN_POINT ( 'NONE',  ( -4.000000000000000000, 0.000000000000000000, 0.000000000000000000 ) ) ;
#5036 = VECTOR ( 'NONE', #5367, 1000.000000000000000 ) ;
#5037 = CARTESIAN_POINT ( 'NONE',  ( -4.000000000000000000, 1.557668341133497059, -0.1596965656957516910 ) ) ;
#5038 = CARTESIAN_POINT ( 'NONE',  ( 49.98886144361676287, 86.06516230458066730, -2.156352803700544385 ) ) ;
#5039 = ORIENTED_EDGE ( 'NONE', *, *, #5399, .F. ) ;
#5040 = B_SPLINE_CURVE_WITH_KNOTS ( 'NONE', 3,
 ( #7753, #153, #4644, #5159 ),
 .UNSPECIFIED., .F., .F.,
 ( 4, 4 ),
 ( 2.380737582494440699E-07, 0.002336974151641604564 ),
 .UNSPECIFIED. ) ;
#5041 = VECTOR ( 'NONE', #4039, 1000.000000000000000 ) ;
#5042 = AXIS2_PLACEMENT_3D ( 'NONE', #576, #6178, #1206 ) ;
#5043 = AXIS2_PLACEMENT_3D ( 'NONE', #923, #7858, #873 ) ;
#5044 = VERTEX_POINT ( 'NONE', #3376 ) ;
#5045 = AXIS2_PLACEMENT_3D ( 'NONE', #3383, #3315, #7634 ) ;
#5046 = CARTESIAN_POINT ( 'NONE',  ( -42.00000000000000711, 85.00000000000011369, 5.000000000000047073 ) ) ;
#5047 = ORIENTED_EDGE ( 'NONE', *, *, #1854, .T. ) ;
#5048 = EDGE_LOOP ( 'NONE', ( #4641, #15 ) ) ;
#5049 = EDGE_CURVE ( 'NONE', #1609, #4874, #7279, .T. ) ;
#5050 = DIRECTION ( 'NONE',  ( 0.000000000000000000, 0.000000000000000000, 1.000000000000000000 ) ) ;
#5051 = DIRECTION ( 'NONE',  ( 0.000000000000000000, 0.000000000000000000, 1.000000000000000000 ) ) ;
#5052 = DIRECTION ( 'NONE',  ( -0.000000000000000000, 1.000000000000000000, -0.000000000000000000 ) ) ;
#5053 = VECTOR ( 'NONE', #4587, 1000.000000000000000 ) ;
#5054 = DIRECTION ( 'NONE',  ( -1.000000000000000000, -3.716747343151140615E-17, -9.918275451135246370E-19 ) ) ;
#5055 = AXIS2_PLACEMENT_3D ( 'NONE', #2717, #5261, #6613 ) ;
#5056 = ORIENTED_EDGE ( 'NONE', *, *, #784, .F. ) ;
#5057 = CARTESIAN_POINT ( 'NONE',  ( -2.000000000000022649, -3.464101615137742396, -2.700000000000001066 ) ) ;
#5058 = ORIENTED_EDGE ( 'NONE', *, *, #2744, .F. ) ;
#5059 = EDGE_CURVE ( 'NONE', #7189, #7486, #3983, .T. ) ;
#5060 = ORIENTED_EDGE ( 'NONE', *, *, #1072, .T. ) ;
#5061 = VECTOR ( 'NONE', #2148, 1000.000000000000000 ) ;
#5062 = CONICAL_SURFACE ( 'NONE', #3727, 4.000000000000000000, 1.047197551196595855 ) ;
#5063 = EDGE_CURVE ( 'NONE', #6340, #5215, #2386, .T. ) ;
#5064 = CARTESIAN_POINT ( 'NONE',  ( 0.000000000000000000, -1.178949249685215417, 2.042000000000002036 ) ) ;
#5065 = FACE_BOUND ( 'NONE', #4199, .T. ) ;
#5066 = DIRECTION ( 'NONE',  ( -0.000000000000000000, -0.000000000000000000, 1.000000000000000000 ) ) ;
#5067 =( LENGTH_UNIT ( ) NAMED_UNIT ( * ) SI_UNIT ( .MILLI., .METRE. ) );
#5068 = PRODUCT ( 'BR-153', 'BR-153', '', ( #4659 ) ) ;
#5069 = COLOUR_RGB ( '', 0.31764706, 0.68627451, 0.89019608) ;
#5070 = CARTESIAN_POINT ( 'NONE',  ( -2.681845249323461911, -6.477919090352733278, 8.004893738113867840 ) ) ;
#5071 = AXIS2_PLACEMENT_3D ( 'NONE', #4270, #4440, #2400 ) ;
#5072 = FACE_OUTER_BOUND ( 'NONE', #543, .T. ) ;
#5073 = AXIS2_PLACEMENT_3D ( 'NONE', #211, #257, #297 ) ;
#5074 = ORIENTED_EDGE ( 'NONE', *, *, #7008, .F. ) ;
#5075 = ORIENTED_EDGE ( 'NONE', *, *, #2709, .F. ) ;
#5076 = ADVANCED_FACE ( 'NONE', ( #7854 ), #913, .T. ) ;
#5077 = FILL_AREA_STYLE_COLOUR ( '', #5283 ) ;
#5078 = CARTESIAN_POINT ( 'NONE',  ( 1.274374112546295138E-14, 85.00000000000017053, 2.000000000000043521 ) ) ;
#5079 = DIRECTION ( 'NONE',  ( 0.000000000000000000, -0.8660254037844390407, -0.4999999999999992784 ) ) ;
#5080 = DIRECTION ( 'NONE',  ( 1.000000000000000000, 0.000000000000000000, 0.000000000000000000 ) ) ;
#5081 = DIRECTION ( 'NONE',  ( 0.000000000000000000, 0.000000000000000000, -1.000000000000000000 ) ) ;
#5082 = CARTESIAN_POINT ( 'NONE',  ( -49.95352446852410822, 87.15616155047288771, -1.065671633021394449 ) ) ;
#5083 = VERTEX_POINT ( 'NONE', #2713 ) ;
#5084 = ADVANCED_FACE ( 'NONE', ( #5291 ), #3448, .F. ) ;
#5085 = CARTESIAN_POINT ( 'NONE',  ( -54.99999999999990052, 10.00000000000000000, 17.64999999999876579 ) ) ;
#5086 = DIRECTION ( 'NONE',  ( 1.000000000000000000, 0.000000000000000000, 0.000000000000000000 ) ) ;
#5087 = DIRECTION ( 'NONE',  ( 1.000000000000000000, 0.000000000000000000, 0.000000000000000000 ) ) ;
#5088 = PLANE ( 'NONE',  #1446 ) ;
#5089 = CARTESIAN_POINT ( 'NONE',  ( 2.000000000000000000, -0.8865213383406690406, 1.535500000000000975 ) ) ;
#5090 = ORIENTED_EDGE ( 'NONE', *, *, #1420, .F. ) ;
#5091 = ORIENTED_EDGE ( 'NONE', *, *, #5651, .T. ) ;
#5092 = CARTESIAN_POINT ( 'NONE',  ( -2.999999999999998668, 35.09008114612887397, 4.000000000000000000 ) ) ;
#5093 = PRODUCT_DEFINITION_CONTEXT ( 'detailed design', #767, 'design' ) ;
#5094 = VERTEX_POINT ( 'NONE', #7229 ) ;
#5095 = AXIS2_PLACEMENT_3D ( 'NONE', #816, #4722, #3395 ) ;
#5096 = VERTEX_POINT ( 'NONE', #1507 ) ;
#5097 = DIRECTION ( 'NONE',  ( 0.000000000000000000, 0.000000000000000000, 1.000000000000000000 ) ) ;
#5098 = DIRECTION ( 'NONE',  ( 0.000000000000000000, -1.000000000000000000, 0.000000000000000000 ) ) ;
#5099 = DIRECTION ( 'NONE',  ( -0.7071067811865335839, 0.000000000000000000, 0.7071067811865614505 ) ) ;
#5100 = DIRECTION ( 'NONE',  ( -1.000000000000000000, -4.775037580134256410E-17, -1.363275510545165866E-18 ) ) ;
#5101 = ORIENTED_EDGE ( 'NONE', *, *, #4168, .F. ) ;
#5102 = EDGE_CURVE ( 'NONE', #4584, #7616, #3194, .T. ) ;
#5103 = VERTEX_POINT ( 'NONE', #5871 ) ;
#5104 = ADVANCED_FACE ( 'NONE', ( #7888, #171, #6489 ), #1594, .F. ) ;
#5105 = EDGE_CURVE ( 'NONE', #5142, #821, #6649, .T. ) ;
#5106 = VERTEX_POINT ( 'NONE', #956 ) ;
#5107 = CARTESIAN_POINT ( 'NONE',  ( 9.020562070449730010E-14, 7.000000000000000000, 8.000000000000058620 ) ) ;
#5108 = CARTESIAN_POINT ( 'NONE',  ( 41.93122500247567075, 87.40257814072478482, -0.06338927685536475953 ) ) ;
#5109 = FACE_OUTER_BOUND ( 'NONE', #1068, .T. ) ;
#5110 = FILL_AREA_STYLE ('',( #3971 ) ) ;
#5111 = DIRECTION ( 'NONE',  ( -1.412205397084881070E-17, 2.775557561562891967E-17, 1.000000000000000000 ) ) ;
#5112 = B_SPLINE_CURVE_WITH_KNOTS ( 'NONE', 3,
 ( #318, #3528, #1535, #7916, #3491, #2907 ),
 .UNSPECIFIED., .F., .F.,
 ( 4, 2, 4 ),
 ( 0.004120275011746849653, 0.005288420935197133549, 0.006456566858647416578 ),
 .UNSPECIFIED. ) ;
#5113 = ORIENTED_EDGE ( 'NONE', *, *, #7984, .F. ) ;
#5114 = FACE_OUTER_BOUND ( 'NONE', #7268, .T. ) ;
#5115 = CARTESIAN_POINT ( 'NONE',  ( -54.99999999999990052, 10.00000000000000000, 15.49999999999877254 ) ) ;
#5116 = CIRCLE ( 'NONE', #7206, 2.649999999999999467 ) ;
#5117 = CARTESIAN_POINT ( 'NONE',  ( 1.300000000000000044, 0.000000000000000000, 1.280000000000000027 ) ) ;
#5118 = AXIS2_PLACEMENT_3D ( 'NONE', #5714, #5218, #6476 ) ;
#5119 = DIRECTION ( 'NONE',  ( -1.000000000000000000, -0.000000000000000000, -0.000000000000000000 ) ) ;
#5120 = CARTESIAN_POINT ( 'NONE',  ( -49.99637443241779522, 85.62167278847331886, -2.323444847100760491 ) ) ;
#5121 = ADVANCED_FACE ( 'NONE', ( #137 ), #7114, .F. ) ;
#5122 = VECTOR ( 'NONE', #107, 1000.000000000000000 ) ;
#5123 = VERTEX_POINT ( 'NONE', #2677 ) ;
#5124 = DIRECTION ( 'NONE',  ( 0.000000000000000000, 0.5000000000000009992, 0.8660254037844380415 ) ) ;
#5125 = DIRECTION ( 'NONE',  ( 0.000000000000000000, 0.8660254037844380415, -0.5000000000000012212 ) ) ;
#5126 = CARTESIAN_POINT ( 'NONE',  ( 0.000000000000000000, 0.000000000000000000, 0.000000000000000000 ) ) ;
#5127 = DIRECTION ( 'NONE',  ( -1.000000000000000000, -0.000000000000000000, -0.000000000000000000 ) ) ;
#5128 = FACE_OUTER_BOUND ( 'NONE', #1929, .T. ) ;
#5129 = VERTEX_POINT ( 'NONE', #3966 ) ;
#5130 = ORIENTED_EDGE ( 'NONE', *, *, #5379, .T. ) ;
#5131 = DIRECTION ( 'NONE',  ( 1.412205397084881070E-17, -2.775557561562891967E-17, -1.000000000000000000 ) ) ;
#5132 = ORIENTED_EDGE ( 'NONE', *, *, #3379, .T. ) ;
#5133 = ORIENTED_EDGE ( 'NONE', *, *, #838, .T. ) ;
#5134 = PRODUCT_DEFINITION_SHAPE ( 'NONE', 'NONE',  #2790 ) ;
#5135 = CARTESIAN_POINT ( 'NONE',  ( 2.500000000000002220, 0.000000000000000000, 0.000000000000000000 ) ) ;
#5136 = DIRECTION ( 'NONE',  ( 0.000000000000000000, 1.000000000000000000, 0.000000000000000000 ) ) ;
#5137 = DIRECTION ( 'NONE',  ( -1.000000000000000000, -0.000000000000000000, -0.000000000000000000 ) ) ;
#5138 = CARTESIAN_POINT ( 'NONE',  ( -64.00000000000000000, 101.0119620251984287, 5.927885619659409472E-15 ) ) ;
#5139 = ADVANCED_FACE ( 'NONE', ( #1544, #4079 ), #4622, .F. ) ;
#5140 = EDGE_LOOP ( 'NONE', ( #300, #7700, #6556 ) ) ;
#5141 = EDGE_CURVE ( 'NONE', #4428, #6175, #1474, .T. ) ;
#5142 = VERTEX_POINT ( 'NONE', #6524 ) ;
#5143 = ORIENTED_EDGE ( 'NONE', *, *, #3053, .T. ) ;
#5144 = CARTESIAN_POINT ( 'NONE',  ( -54.99999999999990052, 10.00000000000000000, 13.34999999999877573 ) ) ;
#5145 = CARTESIAN_POINT ( 'NONE',  ( 41.93694480353849485, 87.30099207916882165, 0.6941923800780209763 ) ) ;
#5146 = DIRECTION ( 'NONE',  ( 0.000000000000000000, 0.000000000000000000, -1.000000000000000000 ) ) ;
#5147 = VECTOR ( 'NONE', #4650, 1000.000000000000000 ) ;
#5148 = DIRECTION ( 'NONE',  ( -1.412205397084881070E-17, 2.775557561562891967E-17, 1.000000000000000000 ) ) ;
#5149 = EDGE_CURVE ( 'NONE', #4852, #7269, #7812, .T. ) ;
#5150 = CARTESIAN_POINT ( 'NONE',  ( 2.000000000000000000, -1.329782007511004727, 0.7677500000000014868 ) ) ;
#5151 = FACE_OUTER_BOUND ( 'NONE', #4802, .T. ) ;
#5152 = DIRECTION ( 'NONE',  ( 0.000000000000000000, 0.000000000000000000, 1.000000000000000000 ) ) ;
#5153 = EDGE_CURVE ( 'NONE', #8100, #590, #2295, .T. ) ;
#5154 = DIRECTION ( 'NONE',  ( 1.000000000000000000, 0.000000000000000000, 0.000000000000000000 ) ) ;
#5155 = LINE ( 'NONE', #3352, #5673 ) ;
#5156 = EDGE_CURVE ( 'NONE', #3168, #189, #6115, .T. ) ;
#5157 = ORIENTED_EDGE ( 'NONE', *, *, #1387, .F. ) ;
#5158 = DIRECTION ( 'NONE',  ( 0.000000000000000000, 0.8660254037844380415, -0.5000000000000009992 ) ) ;
#5159 = CARTESIAN_POINT ( 'NONE',  ( -2.000000000000022649, -3.464101615137742396, -2.700000000000001066 ) ) ;
#5160 = VECTOR ( 'NONE', #6604, 1000.000000000000000 ) ;
#5161 = CARTESIAN_POINT ( 'NONE',  ( 1.318516776095788767, 3.857556137907071747, 2.429570457523002859E-15 ) ) ;
#5162 = PRESENTATION_STYLE_ASSIGNMENT (( #5925 ) ) ;
#5163 = CIRCLE ( 'NONE', #7917, 1.535500000000000087 ) ;
#5164 = ORIENTED_EDGE ( 'NONE', *, *, #6854, .F. ) ;
#5165 = AXIS2_PLACEMENT_3D ( 'NONE', #2672, #80, #2630 ) ;
#5166 = ORIENTED_EDGE ( 'NONE', *, *, #4496, .T. ) ;
#5167 = CARTESIAN_POINT ( 'NONE',  ( -4.000000000000000000, -1.549102112939103826, -2.542104661404059662 ) ) ;
#5168 = AXIS2_PLACEMENT_3D ( 'NONE', #5646, #8125, #8160 ) ;
#5169 = ORIENTED_EDGE ( 'NONE', *, *, #7329, .T. ) ;
#5170 = VECTOR ( 'NONE', #960, 1000.000000000000000 ) ;
#5171 = ORIENTED_EDGE ( 'NONE', *, *, #5402, .T. ) ;
#5172 = CARTESIAN_POINT ( 'NONE',  ( 7.000000000000000000, 8.572527785734883977E-16, 8.033969604113771368 ) ) ;
#5173 = PLANE ( 'NONE',  #7428 ) ;
#5174 = DIRECTION ( 'NONE',  ( 1.412205397084881070E-17, -2.775557561562891967E-17, -1.000000000000000000 ) ) ;
#5175 = DIRECTION ( 'NONE',  ( -3.716747343151140615E-17, 1.000000000000000000, 1.363075293218192124E-18 ) ) ;
#5176 = AXIS2_PLACEMENT_3D ( 'NONE', #2557, #1261, #2506 ) ;
#5177 = VECTOR ( 'NONE', #7915, 1000.000000000000227 ) ;
#5178 = ORIENTED_EDGE ( 'NONE', *, *, #150, .F. ) ;
#5179 = CIRCLE ( 'NONE', #2646, 1.535500000000000087 ) ;
#5180 = EDGE_LOOP ( 'NONE', ( #6309, #3028, #5707, #4148 ) ) ;
#5181 = ORIENTED_EDGE ( 'NONE', *, *, #1184, .T. ) ;
#5182 = ADVANCED_BREP_SHAPE_REPRESENTATION ( '', ( #6686, #1587 ), #1249 ) ;
#5183 = AXIS2_PLACEMENT_3D ( 'NONE', #2338, #4932, #2431 ) ;
#5184 = DIRECTION ( 'NONE',  ( 0.000000000000000000, 0.5000000000000009992, 0.8660254037844381525 ) ) ;
#5185 = ADVANCED_FACE ( 'NONE', ( #7355 ), #912, .T. ) ;
#5186 = CARTESIAN_POINT ( 'NONE',  ( 41.94165275491891265, 87.21379561205887399, -0.9356232805456338175 ) ) ;
#5187 = DIRECTION ( 'NONE',  ( -0.7071067811865335839, 8.659560562355102956E-17, -0.7071067811865614505 ) ) ;
#5188 = EDGE_CURVE ( 'NONE', #5664, #554, #6375, .T. ) ;
#5189 = AXIS2_PLACEMENT_3D ( 'NONE', #5092, #4455, #5663 ) ;
#5190 = CARTESIAN_POINT ( 'NONE',  ( -4.272249441377914181, -5.564160999819695697, 8.012551623441856563 ) ) ;
#5191 = AXIS2_PLACEMENT_3D ( 'NONE', #6600, #2795, #3344 ) ;
#5192 = VECTOR ( 'NONE', #2605, 1000.000000000000000 ) ;
#5193 = VECTOR ( 'NONE', #2401, 1000.000000000000000 ) ;
#5194 = CARTESIAN_POINT ( 'NONE',  ( 4.000000000000003553, 4.286263797015736595E-16, -3.500000000000000000 ) ) ;
#5195 = DIRECTION ( 'NONE',  ( -1.000000000000000000, -0.000000000000000000, -0.000000000000000000 ) ) ;
#5196 = AXIS2_PLACEMENT_3D ( 'NONE', #5538, #7396, #5003 ) ;
#5197 = B_SPLINE_CURVE_WITH_KNOTS ( 'NONE', 3,
 ( #5057, #7101, #2559, #5211, #7726, #1458 ),
 .UNSPECIFIED., .F., .F.,
 ( 4, 2, 4 ),
 ( 0.002336974151641604564, 0.003500975885716477512, 0.004664977619791350026 ),
 .UNSPECIFIED. ) ;
#5198 = CARTESIAN_POINT ( 'NONE',  ( 4.000000000000001776, 2.694222958124178486E-16, 2.200000000000001066 ) ) ;
#5199 = DIRECTION ( 'NONE',  ( 1.000000000000000000, -0.000000000000000000, -0.000000000000000000 ) ) ;
#5200 = ADVANCED_FACE ( 'NONE', ( #5462, #3625 ), #8053, .T. ) ;
#5201 = EDGE_CURVE ( 'NONE', #3227, #2013, #3714, .T. ) ;
#5202 = CIRCLE ( 'NONE', #256, 4.999999999999993783 ) ;
#5203 = EDGE_CURVE ( 'NONE', #3217, #2810, #4870, .T. ) ;
#5204 = ORIENTED_EDGE ( 'NONE', *, *, #1282, .T. ) ;
#5205 = CARTESIAN_POINT ( 'NONE',  ( 2.000000000000000000, -0.8865213383406685965, 1.535500000000000531 ) ) ;
#5206 = FACE_BOUND ( 'NONE', #6072, .T. ) ;
#5207 = AXIS2_PLACEMENT_3D ( 'NONE', #2613, #5154, #7670 ) ;
#5208 = DIRECTION ( 'NONE',  ( 1.000000000000000000, 0.000000000000000000, 0.000000000000000000 ) ) ;
#5209 = CARTESIAN_POINT ( 'NONE',  ( -49.99999999999999289, 85.00000000000005684, 2.400000000000013234 ) ) ;
#5210 = ORIENTED_EDGE ( 'NONE', *, *, #7389, .T. ) ;
#5211 = CARTESIAN_POINT ( 'NONE',  ( -3.344563996438218556, -2.687817229851498624, -2.541324518471498983 ) ) ;
#5212 = EDGE_LOOP ( 'NONE', ( #5819, #2710, #6521, #4411 ) ) ;
#5213 = DIRECTION ( 'NONE',  ( 0.000000000000000000, -0.5000000000000011102, -0.8660254037844379305 ) ) ;
#5214 = ORIENTED_EDGE ( 'NONE', *, *, #5149, .F. ) ;
#5215 = VERTEX_POINT ( 'NONE', #6728 ) ;
#5216 = DIRECTION ( 'NONE',  ( -1.000000000000000000, 0.000000000000000000, -0.000000000000000000 ) ) ;
#5217 = CARTESIAN_POINT ( 'NONE',  ( -1.249999999999992228, 38.99999999999999289, 1.765256746356098409E-17 ) ) ;
#5218 = DIRECTION ( 'NONE',  ( 3.734459788183132523E-17, 2.081668171172168513E-17, 1.000000000000000000 ) ) ;
#5219 = CIRCLE ( 'NONE', #6400, 2.649999999999995914 ) ;
#5220 = VERTEX_POINT ( 'NONE', #1164 ) ;
#5221 = ADVANCED_FACE ( 'NONE', ( #4790 ), #1713, .T. ) ;
#5222 = EDGE_LOOP ( 'NONE', ( #6052, #7612, #1939, #1648, #7998 ) ) ;
#5223 = ORIENTED_EDGE ( 'NONE', *, *, #6504, .T. ) ;
#5224 = CARTESIAN_POINT ( 'NONE',  ( 0.000000000000000000, 0.000000000000000000, 18.00000000000000355 ) ) ;
#5225 = CARTESIAN_POINT ( 'NONE',  ( 41.93238906222617146, 82.61770977831005780, 0.3178396967579638077 ) ) ;
#5226 = DIRECTION ( 'NONE',  ( 0.000000000000000000, -0.5000000000000011102, -0.8660254037844379305 ) ) ;
#5227 = EDGE_CURVE ( 'NONE', #6761, #4663, #1593, .T. ) ;
#5228 = AXIS2_PLACEMENT_3D ( 'NONE', #6703, #5347, #3471 ) ;
#5229 = DIRECTION ( 'NONE',  ( 0.000000000000000000, 0.000000000000000000, 1.000000000000000000 ) ) ;
#5230 = LINE ( 'NONE', #3982, #2924 ) ;
#5231 = DIRECTION ( 'NONE',  ( -0.000000000000000000, -0.000000000000000000, 1.000000000000000000 ) ) ;
#5232 = EDGE_CURVE ( 'NONE', #402, #3653, #4763, .T. ) ;
#5233 = STYLED_ITEM ( 'NONE', ( #5956 ), #4869 ) ;
#5234 = CARTESIAN_POINT ( 'NONE',  ( -49.99926415638493893, 85.31227754079897352, -2.384817760534238218 ) ) ;
#5235 = EDGE_CURVE ( 'NONE', #3008, #4266, #5833, .T. ) ;
#5236 = EDGE_LOOP ( 'NONE', ( #1090, #4397, #2436, #2711 ) ) ;
#5237 = FACE_BOUND ( 'NONE', #1295, .T. ) ;
#5238 = DIRECTION ( 'NONE',  ( 0.000000000000000000, 1.000000000000000000, 0.000000000000000000 ) ) ;
#5239 = DIRECTION ( 'NONE',  ( 0.000000000000000000, -1.000000000000000000, 0.000000000000000000 ) ) ;
#5240 = COLOUR_RGB ( '', 0.72549020, 0.75294118, 0.79215686) ;
#5241 = DIRECTION ( 'NONE',  ( 0.000000000000000000, 0.000000000000000000, 1.000000000000000000 ) ) ;
#5242 = PRODUCT_RELATED_PRODUCT_CATEGORY ( 'part', '', ( #8089 ) ) ;
#5243 = CARTESIAN_POINT ( 'NONE',  ( -50.00000000000000000, 84.84140190613180721, 2.399999999999987921 ) ) ;
#5244 = EDGE_LOOP ( 'NONE', ( #673, #7650, #1470, #2486 ) ) ;
#5245 = CARTESIAN_POINT ( 'NONE',  ( 52.00000000000000711, 8.000000000000000000, -8.000000000000000000 ) ) ;
#5246 = ORIENTED_EDGE ( 'NONE', *, *, #309, .F. ) ;
#5247 = VERTEX_POINT ( 'NONE', #1083 ) ;
#5248 = LINE ( 'NONE', #274, #7678 ) ;
#5249 = DIRECTION ( 'NONE',  ( 0.000000000000000000, 0.000000000000000000, -1.000000000000000000 ) ) ;
#5250 = DIRECTION ( 'NONE',  ( 0.8191520442889896891, 0.000000000000000000, 0.5735764363510490460 ) ) ;
#5251 = ORIENTED_EDGE ( 'NONE', *, *, #4592, .F. ) ;
#5252 = ORIENTED_EDGE ( 'NONE', *, *, #201, .F. ) ;
#5253 = UNCERTAINTY_MEASURE_WITH_UNIT (LENGTH_MEASURE( 1.000000000000000082E-05 ), #2108, 'distance_accuracy_value', 'NONE');
#5254 = VERTEX_POINT ( 'NONE', #3586 ) ;
#5255 = ADVANCED_FACE ( 'NONE', ( #2330 ), #6148, .F. ) ;
#5256 = CARTESIAN_POINT ( 'NONE',  ( -31.74999999999994316, 5.204748896376250699E-16, -4.250000000000000000 ) ) ;
#5257 = DIRECTION ( 'NONE',  ( -0.000000000000000000, -0.000000000000000000, 1.000000000000000000 ) ) ;
#5258 = CYLINDRICAL_SURFACE ( 'NONE', #2216, 1.500000000000000222 ) ;
#5259 = SURFACE_SIDE_STYLE ('',( #1435 ) ) ;
#5260 = CARTESIAN_POINT ( 'NONE',  ( 2.500000000000002220, 2.357898499370434386, -3.469446951953614189E-15 ) ) ;
#5261 = DIRECTION ( 'NONE',  ( -1.000000000000000000, 0.000000000000000000, 0.000000000000000000 ) ) ;
#5262 = AXIS2_PLACEMENT_3D ( 'NONE', #1414, #7530, #3183 ) ;
#5263 = CARTESIAN_POINT ( 'NONE',  ( 2.500000000000015987, -1.768423874527823347, -1.020999999999997687 ) ) ;
#5264 = CARTESIAN_POINT ( 'NONE',  ( 1.284259550325887758E-14, 85.00000000000005684, -5.000000000000004441 ) ) ;
#5265 = CARTESIAN_POINT ( 'NONE',  ( 2.000000000000000000, 0.000000000000000000, 0.000000000000000000 ) ) ;
#5266 = AXIS2_PLACEMENT_3D ( 'NONE', #5811, #2040, #5855 ) ;
#5267 = AXIS2_PLACEMENT_3D ( 'NONE', #1618, #1021, #3564 ) ;
#5268 = EDGE_LOOP ( 'NONE', ( #4385, #7546, #6119, #5214 ) ) ;
#5269 = LINE ( 'NONE', #4760, #7629 ) ;
#5270 = ADVANCED_FACE ( 'NONE', ( #7444 ), #7285, .F. ) ;
#5271 = SURFACE_SIDE_STYLE ('',( #5887 ) ) ;
#5272 = DIRECTION ( 'NONE',  ( 1.000000000000000000, 0.000000000000000000, 0.000000000000000000 ) ) ;
#5273 = EDGE_CURVE ( 'NONE', #4939, #1235, #3667, .T. ) ;
#5274 = DIRECTION ( 'NONE',  ( 1.000000000000000000, 0.000000000000000000, 0.000000000000000000 ) ) ;
#5275 = EDGE_CURVE ( 'NONE', #5642, #6175, #5586, .T. ) ;
#5276 = FACE_OUTER_BOUND ( 'NONE', #2943, .T. ) ;
#5277 = ORIENTED_EDGE ( 'NONE', *, *, #6204, .F. ) ;
#5278 = CARTESIAN_POINT ( 'NONE',  ( 49.99923958211703479, 84.68425784446333182, 2.384302390493924673 ) ) ;
#5279 = ORIENTED_EDGE ( 'NONE', *, *, #7859, .T. ) ;
#5280 = EDGE_LOOP ( 'NONE', ( #2980, #1808, #4586, #1571 ) ) ;
#5281 = VECTOR ( 'NONE', #20, 1000.000000000000114 ) ;
#5282 = DIRECTION ( 'NONE',  ( 0.000000000000000000, 1.000000000000000000, 0.000000000000000000 ) ) ;
#5283 = COLOUR_RGB ( '', 0.40784314, 0.44705882, 0.49803922) ;
#5284 = CARTESIAN_POINT ( 'NONE',  ( 52.00000000000000000, 7.999999999999996447, 11.99999999999998934 ) ) ;
#5285 = DIRECTION ( 'NONE',  ( 0.000000000000000000, 0.000000000000000000, 1.000000000000000000 ) ) ;
#5286 = MECHANICAL_DESIGN_GEOMETRIC_PRESENTATION_REPRESENTATION (  '', ( #213 ), #94 ) ;
#5287 = ORIENTED_EDGE ( 'NONE', *, *, #3787, .F. ) ;
#5288 = EDGE_LOOP ( 'NONE', ( #1393, #1942 ) ) ;
#5289 = VERTEX_POINT ( 'NONE', #324 ) ;
#5290 = VECTOR ( 'NONE', #1794, 1000.000000000000227 ) ;
#5291 = FACE_OUTER_BOUND ( 'NONE', #7443, .T. ) ;
#5292 = CARTESIAN_POINT ( 'NONE',  ( 2.889328000935821095, -6.379995247853900153, 8.005756244325109350 ) ) ;
#5293 = CARTESIAN_POINT ( 'NONE',  ( -31.74999999999995737, 0.000000000000000000, 0.000000000000000000 ) ) ;
#5294 = AXIS2_PLACEMENT_3D ( 'NONE', #7464, #5558, #1869 ) ;
#5295 = AXIS2_PLACEMENT_3D ( 'NONE', #1218, #2595, #2462 ) ;
#5296 = FILL_AREA_STYLE ('',( #5949 ) ) ;
#5297 = EDGE_LOOP ( 'NONE', ( #8007, #1203, #3842, #75, #182 ) ) ;
#5298 = FILL_AREA_STYLE ('',( #4743 ) ) ;
#5299 = VECTOR ( 'NONE', #2823, 1000.000000000000114 ) ;
#5300 = EDGE_CURVE ( 'NONE', #3653, #402, #5842, .T. ) ;
#5301 = VECTOR ( 'NONE', #4480, 999.9999999999998863 ) ;
#5302 = AXIS2_PLACEMENT_3D ( 'NONE', #8083, #6926, #6964 ) ;
#5303 = CARTESIAN_POINT ( 'NONE',  ( 2.999999999999999112, 45.09008114612887397, 4.000000000000000000 ) ) ;
#5304 = CARTESIAN_POINT ( 'NONE',  ( 30.00000000000000000, 0.000000000000000000, -6.938893903907228378E-15 ) ) ;
#5305 = VECTOR ( 'NONE', #5563, 1000.000000000000000 ) ;
#5306 = AXIS2_PLACEMENT_3D ( 'NONE', #455, #2916, #7395 ) ;
#5307 = FACE_OUTER_BOUND ( 'NONE', #1447, .T. ) ;
#5308 = AXIS2_PLACEMENT_3D ( 'NONE', #3940, #7124, #3197 ) ;
#5309 = CARTESIAN_POINT ( 'NONE',  ( 60.00000000000000711, 9.332579536216795825E-15, 54.99999999999997868 ) ) ;
#5310 = ADVANCED_FACE ( 'NONE', ( #3537 ), #5710, .F. ) ;
#5311 = VERTEX_POINT ( 'NONE', #546 ) ;
#5312 = LINE ( 'NONE', #7831, #591 ) ;
#5313 = TOROIDAL_SURFACE ( 'NONE', #532, 2.600000000000000089, 0.1499999999999999944 ) ;
#5314 = CARTESIAN_POINT ( 'NONE',  ( 2.339468227445713477, 3.268109542640643905, -2.700000000000003286 ) ) ;
#5315 = DIRECTION ( 'NONE',  ( -0.000000000000000000, 1.000000000000000000, -0.000000000000000000 ) ) ;
#5316 = DIRECTION ( 'NONE',  ( 0.000000000000000000, 0.000000000000000000, -1.000000000000000000 ) ) ;
#5317 = LINE ( 'NONE', #6282, #2261 ) ;
#5318 = FACE_OUTER_BOUND ( 'NONE', #4381, .T. ) ;
#5319 = DIRECTION ( 'NONE',  ( 1.412205397084881070E-17, -2.775557561562891967E-17, -1.000000000000000000 ) ) ;
#5320 = VERTEX_POINT ( 'NONE', #7617 ) ;
#5321 = CIRCLE ( 'NONE', #925, 1.649999999999984812 ) ;
#5322 = CARTESIAN_POINT ( 'NONE',  ( 2.000000000000000000, 1.880445160090761061E-16, -1.535500000000000087 ) ) ;
#5323 = PRODUCT_DEFINITION_CONTEXT ( 'detailed design', #2796, 'design' ) ;
#5324 = EDGE_CURVE ( 'NONE', #1081, #5786, #3324, .T. ) ;
#5325 = ORIENTED_EDGE ( 'NONE', *, *, #643, .F. ) ;
#5326 = ORIENTED_EDGE ( 'NONE', *, *, #1402, .T. ) ;
#5327 = MECHANICAL_DESIGN_GEOMETRIC_PRESENTATION_REPRESENTATION (  '', ( #2134 ), #5728 ) ;
#5328 = FACE_OUTER_BOUND ( 'NONE', #588, .T. ) ;
#5329 = CARTESIAN_POINT ( 'NONE',  ( 57.99999999999999289, -8.000000000000003553, 11.99999999999998934 ) ) ;
#5330 = CARTESIAN_POINT ( 'NONE',  ( -60.00000000000000000, 10.00000000000000000, 20.00000000000000355 ) ) ;
#5331 = CYLINDRICAL_SURFACE ( 'NONE', #3690, 42.00000000000002132 ) ;
#5332 = ORIENTED_EDGE ( 'NONE', *, *, #6688, .F. ) ;
#5333 = ORIENTED_EDGE ( 'NONE', *, *, #6253, .F. ) ;
#5334 = ORIENTED_EDGE ( 'NONE', *, *, #5836, .F. ) ;
#5335 = DIRECTION ( 'NONE',  ( 1.000000000000000000, 0.000000000000000000, 0.000000000000000000 ) ) ;
#5336 = DIRECTION ( 'NONE',  ( 0.000000000000000000, 0.000000000000000000, -1.000000000000000000 ) ) ;
#5337 = FACE_OUTER_BOUND ( 'NONE', #1395, .T. ) ;
#5338 =( NAMED_UNIT ( * ) PLANE_ANGLE_UNIT ( ) SI_UNIT ( $, .RADIAN. ) );
#5339 = ADVANCED_FACE ( 'NONE', ( #3130 ), #3800, .F. ) ;
#5340 = CARTESIAN_POINT ( 'NONE',  ( 4.000000000000003553, 0.000000000000000000, 0.000000000000000000 ) ) ;
#5341 = ADVANCED_FACE ( 'NONE', ( #5788 ), #8180, .F. ) ;
#5342 = CIRCLE ( 'NONE', #7850, 0.1499999999999999667 ) ;
#5343 = CARTESIAN_POINT ( 'NONE',  ( -39.00000000000000711, 85.00000000000017053, 2.000000000000043077 ) ) ;
#5344 = DIRECTION ( 'NONE',  ( 0.000000000000000000, 0.000000000000000000, 1.000000000000000000 ) ) ;
#5345 = DIRECTION ( 'NONE',  ( 0.000000000000000000, 0.000000000000000000, 1.000000000000000000 ) ) ;
#5346 = APPLICATION_CONTEXT ( 'automotive_design' ) ;
#5347 = DIRECTION ( 'NONE',  ( 0.000000000000000000, 0.000000000000000000, -1.000000000000000000 ) ) ;
#5348 = ORIENTED_EDGE ( 'NONE', *, *, #3930, .T. ) ;
#5349 = ORIENTED_EDGE ( 'NONE', *, *, #6854, .T. ) ;
#5350 = FACE_OUTER_BOUND ( 'NONE', #122, .T. ) ;
#5351 = EDGE_CURVE ( 'NONE', #5475, #471, #4458, .T. ) ;
#5352 = DIRECTION ( 'NONE',  ( -0.000000000000000000, 0.000000000000000000, 1.000000000000000000 ) ) ;
#5353 = DIRECTION ( 'NONE',  ( 0.000000000000000000, 0.4999999999999991673, -0.8660254037844391517 ) ) ;
#5354 = DIRECTION ( 'NONE',  ( -1.000000000000000000, 0.000000000000000000, 0.000000000000000000 ) ) ;
#5355 = DIRECTION ( 'NONE',  ( 1.412205397084881070E-17, -2.775557561562891967E-17, -1.000000000000000000 ) ) ;
#5356 = CARTESIAN_POINT ( 'NONE',  ( 50.00000000000000000, -10.00000000000000000, 60.00000000000000000 ) ) ;
#5357 = EDGE_CURVE ( 'NONE', #5862, #4997, #7967, .T. ) ;
#5358 = ADVANCED_FACE ( 'NONE', ( #8143 ), #3220, .F. ) ;
#5359 = LINE ( 'NONE', #1493, #3084 ) ;
#5360 = ORIENTED_EDGE ( 'NONE', *, *, #643, .T. ) ;
#5361 = CARTESIAN_POINT ( 'NONE',  ( 3.000000000000000000, 1.959434878635765477E-16, 1.600000000000000311 ) ) ;
#5362 = EDGE_LOOP ( 'NONE', ( #1020, #7693 ) ) ;
#5363 = ORIENTED_EDGE ( 'NONE', *, *, #241, .T. ) ;
#5364 = FACE_OUTER_BOUND ( 'NONE', #301, .T. ) ;
#5365 = CARTESIAN_POINT ( 'NONE',  ( 4.000000000000003553, 1.557668341133516154, -2.540303434304242547 ) ) ;
#5366 = CARTESIAN_POINT ( 'NONE',  ( 0.000000000000000000, 0.000000000000000000, 0.000000000000000000 ) ) ;
#5367 = DIRECTION ( 'NONE',  ( 0.000000000000000000, 0.4999999999999991118, -0.8660254037844391517 ) ) ;
#5368 = FILL_AREA_STYLE ('',( #4822 ) ) ;
#5369 = SHAPE_DEFINITION_REPRESENTATION ( #1124, #7239 ) ;
#5370 = VERTEX_POINT ( 'NONE', #5172 ) ;
#5371 = ORIENTED_EDGE ( 'NONE', *, *, #3146, .F. ) ;
#5372 = VERTEX_POINT ( 'NONE', #3174 ) ;
#5373 = AXIS2_PLACEMENT_3D ( 'NONE', #5032, #7640, #6310 ) ;
#5374 = DIRECTION ( 'NONE',  ( -1.000000000000000000, 0.000000000000000000, 0.000000000000000000 ) ) ;
#5375 = ADVANCED_FACE ( 'NONE', ( #585 ), #5002, .T. ) ;
#5376 = DIRECTION ( 'NONE',  ( 0.000000000000000000, -0.5000000000000009992, -0.8660254037844380415 ) ) ;
#5377 = DIRECTION ( 'NONE',  ( 0.000000000000000000, -1.000000000000000000, 1.100686371591861952E-15 ) ) ;
#5378 = SURFACE_STYLE_USAGE ( .BOTH. , #7891 ) ;
#5379 = EDGE_CURVE ( 'NONE', #2810, #4315, #8066, .T. ) ;
#5380 = DIRECTION ( 'NONE',  ( 1.000000000000000000, 0.000000000000000000, 0.000000000000000000 ) ) ;
#5381 = CARTESIAN_POINT ( 'NONE',  ( -1.660531772554312724, 3.660093687634849324, 2.664342135588401717E-15 ) ) ;
#5382 = CARTESIAN_POINT ( 'NONE',  ( -39.83716857408418122, 108.0000000000001421, 4.163336342344337027E-14 ) ) ;
#5383 = DIRECTION ( 'NONE',  ( 1.000000000000000000, 0.000000000000000000, 0.000000000000000000 ) ) ;
#5384 = FACE_OUTER_BOUND ( 'NONE', #3863, .T. ) ;
#5385 = EDGE_CURVE ( 'NONE', #5096, #5489, #7577, .T. ) ;
#5386 = VERTEX_POINT ( 'NONE', #3760 ) ;
#5387 = VERTEX_POINT ( 'NONE', #1300 ) ;
#5388 = DIRECTION ( 'NONE',  ( 1.000000000000000000, 0.000000000000000000, 0.000000000000000000 ) ) ;
#5389 = EDGE_CURVE ( 'NONE', #1156, #3623, #6472, .T. ) ;
#5390 = PLANE ( 'NONE',  #4881 ) ;
#5391 = DIRECTION ( 'NONE',  ( 1.000000000000000000, 0.000000000000000000, 0.000000000000000000 ) ) ;
#5392 = CARTESIAN_POINT ( 'NONE',  ( -41.98256188053843374, 86.22727746334254562, -2.078089480949581791 ) ) ;
#5393 = DIRECTION ( 'NONE',  ( 1.000000000000000000, 0.000000000000000000, 0.000000000000000000 ) ) ;
#5394 = CARTESIAN_POINT ( 'NONE',  ( -49.96737414687251544, 83.19055800108179710, -1.584620125916080369 ) ) ;
#5395 = CARTESIAN_POINT ( 'NONE',  ( 7.000000000000000000, 8.572527594031473190E-16, 18.00000000000000355 ) ) ;
#5396 = ORIENTED_EDGE ( 'NONE', *, *, #271, .T. ) ;
#5397 = LINE ( 'NONE', #853, #2204 ) ;
#5398 = AXIS2_PLACEMENT_3D ( 'NONE', #3523, #3447, #312 ) ;
#5399 = EDGE_CURVE ( 'NONE', #479, #7219, #7028, .T. ) ;
#5400 = ORIENTED_EDGE ( 'NONE', *, *, #551, .F. ) ;
#5401 = VERTEX_POINT ( 'NONE', #3255 ) ;
#5402 = EDGE_CURVE ( 'NONE', #1419, #4570, #6371, .T. ) ;
#5403 = LINE ( 'NONE', #7345, #4372 ) ;
#5404 = DIRECTION ( 'NONE',  ( -1.000000000000000000, -0.000000000000000000, -0.000000000000000000 ) ) ;
#5405 = CARTESIAN_POINT ( 'NONE',  ( 10.71950000000001424, 0.000000000000000000, 1.500000000000000222 ) ) ;
#5406 = DIRECTION ( 'NONE',  ( -1.000000000000000000, -0.000000000000000000, -0.000000000000000000 ) ) ;
#5407 = PRESENTATION_STYLE_ASSIGNMENT (( #8005 ) ) ;
#5408 = APPLICATION_PROTOCOL_DEFINITION ( 'draft international standard', 'automotive_design', 1998, #2796 ) ;
#5409 = ORIENTED_EDGE ( 'NONE', *, *, #1402, .F. ) ;
#5410 = ORIENTED_EDGE ( 'NONE', *, *, #4829, .F. ) ;
#5411 = VERTEX_POINT ( 'NONE', #6242 ) ;
#5412 = DIRECTION ( 'NONE',  ( 1.000000000000000000, 0.000000000000000000, 0.000000000000000000 ) ) ;
#5413 = DIRECTION ( 'NONE',  ( 0.000000000000000000, -1.000000000000000000, 0.000000000000000000 ) ) ;
#5414 = FACE_OUTER_BOUND ( 'NONE', #5140, .T. ) ;
#5415 = AXIS2_PLACEMENT_3D ( 'NONE', #4390, #1982, #2566 ) ;
#5416 = CIRCLE ( 'NONE', #359, 2.041999999999999815 ) ;
#5417 = ORIENTED_EDGE ( 'NONE', *, *, #5201, .T. ) ;
#5418 = FACE_OUTER_BOUND ( 'NONE', #6210, .T. ) ;
#5419 = AXIS2_PLACEMENT_3D ( 'NONE', #2546, #5127, #3120 ) ;
#5420 = VECTOR ( 'NONE', #7844, 1000.000000000000000 ) ;
#5421 = CARTESIAN_POINT ( 'NONE',  ( -4.000000000000000000, 2.309401076758531346, -2.342734410091827701 ) ) ;
#5422 = CARTESIAN_POINT ( 'NONE',  ( 5.000000000000018652, 3.306546357697858171E-16, 2.699999999999997069 ) ) ;
#5423 = AXIS2_PLACEMENT_3D ( 'NONE', #4500, #1220, #1972 ) ;
#5424 = DIRECTION ( 'NONE',  ( 1.412205397084880761E-17, 2.775557561562891967E-17, 1.000000000000000000 ) ) ;
#5425 = VECTOR ( 'NONE', #1622, 1000.000000000000000 ) ;
#5426 = CARTESIAN_POINT ( 'NONE',  ( 7.000000000000000000, 8.572527785734883977E-16, 8.033969604113771368 ) ) ;
#5427 = VECTOR ( 'NONE', #6123, 1000.000000000000000 ) ;
#5428 = AXIS2_PLACEMENT_3D ( 'NONE', #7050, #2687, #1366 ) ;
#5429 = ORIENTED_EDGE ( 'NONE', *, *, #752, .F. ) ;
#5430 = ORIENTED_EDGE ( 'NONE', *, *, #7037, .T. ) ;
#5431 = DIRECTION ( 'NONE',  ( 0.000000000000000000, 0.000000000000000000, -1.000000000000000000 ) ) ;
#5432 = DIRECTION ( 'NONE',  ( -1.000000000000000000, 0.000000000000000000, 0.000000000000000000 ) ) ;
#5433 = LINE ( 'NONE', #7333, #2478 ) ;
#5434 = VECTOR ( 'NONE', #4552, 1000.000000000000000 ) ;
#5435 = CARTESIAN_POINT ( 'NONE',  ( -41.96090147793647418, 86.81773748145498359, -1.587618400554034359 ) ) ;
#5436 = DIRECTION ( 'NONE',  ( 0.000000000000000000, -0.4999999999999992784, 0.8660254037844390407 ) ) ;
#5437 = DIRECTION ( 'NONE',  ( 1.000000000000000000, 0.000000000000000000, 0.000000000000000000 ) ) ;
#5438 = CIRCLE ( 'NONE', #4639, 4.999999999999997335 ) ;
#5439 = LINE ( 'NONE', #6056, #694 ) ;
#5440 = ORIENTED_EDGE ( 'NONE', *, *, #4341, .F. ) ;
#5441 = ADVANCED_FACE ( 'NONE', ( #4375 ), #2764, .T. ) ;
#5442 = VECTOR ( 'NONE', #3216, 1000.000000000000000 ) ;
#5443 = PLANE ( 'NONE',  #2335 ) ;
#5444 = ADVANCED_FACE ( 'NONE', ( #1892 ), #4579, .F. ) ;
#5445 = EDGE_CURVE ( 'NONE', #8139, #4887, #1463, .T. ) ;
#5446 = ORIENTED_EDGE ( 'NONE', *, *, #2430, .T. ) ;
#5447 = ORIENTED_EDGE ( 'NONE', *, *, #50, .F. ) ;
#5448 = VECTOR ( 'NONE', #1412, 1000.000000000000114 ) ;
#5449 = LINE ( 'NONE', #481, #3707 ) ;
#5450 = DIRECTION ( 'NONE',  ( -0.000000000000000000, -0.000000000000000000, 1.000000000000000000 ) ) ;
#5451 = CYLINDRICAL_SURFACE ( 'NONE', #7603, 1.649999999999995248 ) ;
#5452 = CARTESIAN_POINT ( 'NONE',  ( 0.000000000000000000, 0.000000000000000000, 0.000000000000000000 ) ) ;
#5453 = CARTESIAN_POINT ( 'NONE',  ( 27.35000000000001208, -29.99999999999997868, 10.00000000000000000 ) ) ;
#5454 =( GEOMETRIC_REPRESENTATION_CONTEXT ( 3 ) GLOBAL_UNCERTAINTY_ASSIGNED_CONTEXT ( ( #7942 ) ) GLOBAL_UNIT_ASSIGNED_CONTEXT ( ( #5802, #92, #5765 ) ) REPRESENTATION_CONTEXT ( 'NONE', 'WORKASPACE' ) );
#5455 = CONTEXT_DEPENDENT_SHAPE_REPRESENTATION ( #3317, #1272 ) ;
#5456 = VECTOR ( 'NONE', #6149, 1000.000000000000114 ) ;
#5457 = AXIS2_PLACEMENT_3D ( 'NONE', #4526, #5231, #29 ) ;
#5458 = ORIENTED_EDGE ( 'NONE', *, *, #7301, .F. ) ;
#5459 = VERTEX_POINT ( 'NONE', #194 ) ;
#5460 = ORIENTED_EDGE ( 'NONE', *, *, #2876, .T. ) ;
#5461 = B_SPLINE_CURVE_WITH_KNOTS ( 'NONE', 3,
 ( #6403, #4540, #5167, #2012, #7064, #3917 ),
 .UNSPECIFIED., .F., .F.,
 ( 4, 2, 4 ),
 ( 0.004120275011746843581, 0.005288420935197119671, 0.006456566858647395761 ),
 .UNSPECIFIED. ) ;
#5462 = FACE_OUTER_BOUND ( 'NONE', #4098, .T. ) ;
#5463 = LINE ( 'NONE', #2917, #1202 ) ;
#5464 = DIRECTION ( 'NONE',  ( 0.000000000000000000, -0.5000000000000008882, -0.8660254037844380415 ) ) ;
#5465 = EDGE_LOOP ( 'NONE', ( #6436, #321, #5349, #6941, #6982 ) ) ;
#5466 = ADVANCED_FACE ( 'NONE', ( #6517, #903 ), #6441, .T. ) ;
#5467 = CARTESIAN_POINT ( 'NONE',  ( 32.64999999999997726, 30.00000000000001421, 10.00000000000000000 ) ) ;
#5468 = ORIENTED_EDGE ( 'NONE', *, *, #7946, .T. ) ;
#5469 = ADVANCED_FACE ( 'NONE', ( #5865 ), #235, .F. ) ;
#5470 = DIRECTION ( 'NONE',  ( -0.000000000000000000, -0.000000000000000000, 1.000000000000000000 ) ) ;
#5471 = DIRECTION ( 'NONE',  ( 1.412205397084881070E-17, -2.775557561562891967E-17, -1.000000000000000000 ) ) ;
#5472 =( NAMED_UNIT ( * ) PLANE_ANGLE_UNIT ( ) SI_UNIT ( $, .RADIAN. ) );
#5473 = CARTESIAN_POINT ( 'NONE',  ( 0.000000000000000000, 1.178949249685218970, 2.041999999999998483 ) ) ;
#5474 = FACE_OUTER_BOUND ( 'NONE', #2130, .T. ) ;
#5475 = VERTEX_POINT ( 'NONE', #1423 ) ;
#5476 = ORIENTED_EDGE ( 'NONE', *, *, #8182, .T. ) ;
#5477 = DIRECTION ( 'NONE',  ( 0.000000000000000000, -0.000000000000000000, 1.000000000000000000 ) ) ;
#5478 = DIRECTION ( 'NONE',  ( 0.8571673007021125557, 2.194743421410585277E-16, -0.5150380749100536004 ) ) ;
#5479 = CARTESIAN_POINT ( 'NONE',  ( -41.93504501509995919, 87.33507146524520692, 0.5690079308734952157 ) ) ;
#5480 = CARTESIAN_POINT ( 'NONE',  ( 0.000000000000000000, -0.7390083445627200209, 1.280000000000001137 ) ) ;
#5481 = EDGE_CURVE ( 'NONE', #3297, #939, #7266, .T. ) ;
#5482 = CARTESIAN_POINT ( 'NONE',  ( -49.94237215279110131, 82.60011171831004617, 0.3139783802610798258 ) ) ;
#5483 = VECTOR ( 'NONE', #258, 1000.000000000000000 ) ;
#5484 = LINE ( 'NONE', #2940, #5840 ) ;
#5485 = EDGE_CURVE ( 'NONE', #7927, #6791, #2370, .T. ) ;
#5486 = ORIENTED_EDGE ( 'NONE', *, *, #7922, .F. ) ;
#5487 = CARTESIAN_POINT ( 'NONE',  ( 60.00000000000000711, 10.00000000000000000, 60.00000000000000000 ) ) ;
#5488 = ORIENTED_EDGE ( 'NONE', *, *, #3911, .T. ) ;
#5489 = VERTEX_POINT ( 'NONE', #7762 ) ;
#5490 = FACE_OUTER_BOUND ( 'NONE', #8021, .T. ) ;
#5491 = CARTESIAN_POINT ( 'NONE',  ( 2.500000000000002220, 2.357898499370434386, -3.469446951953614189E-15 ) ) ;
#5492 = CARTESIAN_POINT ( 'NONE',  ( 1.300000000000000044, 1.478016689125442484, -1.626303258728256651E-15 ) ) ;
#5493 = CARTESIAN_POINT ( 'NONE',  ( -0.9176763012970977629, 6.954530811262681134, 8.000445331782056968 ) ) ;
#5494 = EDGE_LOOP ( 'NONE', ( #999, #4245, #4025, #6511 ) ) ;
#5495 = ORIENTED_EDGE ( 'NONE', *, *, #2192, .F. ) ;
#5496 = EDGE_LOOP ( 'NONE', ( #5896, #2625 ) ) ;
#5497 = CARTESIAN_POINT ( 'NONE',  ( 0.000000000000000000, 0.000000000000000000, -2.700000000000001066 ) ) ;
#5498 = CYLINDRICAL_SURFACE ( 'NONE', #5196, 4.999999999999993783 ) ;
#5499 = EDGE_CURVE ( 'NONE', #4127, #493, #1536, .T. ) ;
#5500 = CARTESIAN_POINT ( 'NONE',  ( -2.999999999999998668, 35.09008114612887397, 0.000000000000000000 ) ) ;
#5501 =( GEOMETRIC_REPRESENTATION_CONTEXT ( 3 ) GLOBAL_UNCERTAINTY_ASSIGNED_CONTEXT ( ( #7792 ) ) GLOBAL_UNIT_ASSIGNED_CONTEXT ( ( #6154, #6780, #6734 ) ) REPRESENTATION_CONTEXT ( 'NONE', 'WORKASPACE' ) );
#5502 = FILL_AREA_STYLE_COLOUR ( '', #6678 ) ;
#5503 = EDGE_LOOP ( 'NONE', ( #162, #6113 ) ) ;
#5504 = DIRECTION ( 'NONE',  ( 0.000000000000000000, 0.8660254037844380415, -0.5000000000000012212 ) ) ;
#5505 = ORIENTED_EDGE ( 'NONE', *, *, #4527, .F. ) ;
#5506 = AXIS2_PLACEMENT_3D ( 'NONE', #5205, #5158, #5124 ) ;
#5507 = EDGE_CURVE ( 'NONE', #3305, #554, #3369, .T. ) ;
#5508 = EDGE_LOOP ( 'NONE', ( #1633, #8028, #5488, #7972 ) ) ;
#5509 = DIRECTION ( 'NONE',  ( 1.000000000000000000, 0.000000000000000000, 0.000000000000000000 ) ) ;
#5510 = DIRECTION ( 'NONE',  ( -0.000000000000000000, 0.000000000000000000, -1.000000000000000000 ) ) ;
#5511 = SHAPE_REPRESENTATION_RELATIONSHIP ( 'NONE' , 'NONE' ,  #6413, #5182 ) ;
#5512 = PRODUCT ( 'hex thin nut chamfered gradeab_iso_ISO - 4035 - M5 - N', 'hex thin nut chamfered gradeab_iso_ISO - 4035 - M5 - N', '', ( #7185 ) ) ;
#5513 = CARTESIAN_POINT ( 'NONE',  ( 0.000000000000000000, 0.7390083445627193548, -1.280000000000000693 ) ) ;
#5514 = CARTESIAN_POINT ( 'NONE',  ( -31.74999999999995737, 4.286263797015736595E-16, -3.500000000000000000 ) ) ;
#5515 = ORIENTED_EDGE ( 'NONE', *, *, #7516, .T. ) ;
#5516 = ORIENTED_EDGE ( 'NONE', *, *, #291, .T. ) ;
#5517 = FACE_OUTER_BOUND ( 'NONE', #3073, .T. ) ;
#5518 = LINE ( 'NONE', #4765, #6908 ) ;
#5519 = CARTESIAN_POINT ( 'NONE',  ( -42.00000000000000711, 85.00000000000011369, 5.000000000000047073 ) ) ;
#5520 = CARTESIAN_POINT ( 'NONE',  ( 0.000000000000000000, 0.000000000000000000, 0.000000000000000000 ) ) ;
#5521 = CARTESIAN_POINT ( 'NONE',  ( -10.00000000000000000, 0.000000000000000000, 10.00000000000000000 ) ) ;
#5522 = VERTEX_POINT ( 'NONE', #2160 ) ;
#5523 = EDGE_CURVE ( 'NONE', #397, #6761, #6607, .T. ) ;
#5524 = VERTEX_POINT ( 'NONE', #2085 ) ;
#5525 = CARTESIAN_POINT ( 'NONE',  ( 1.660531772554324048, -3.660093687634887516, -2.070868501094675553E-14 ) ) ;
#5526 = ADVANCED_FACE ( 'NONE', ( #7143 ), #4006, .T. ) ;
#5527 = DIRECTION ( 'NONE',  ( 1.000000000000000000, 0.000000000000000000, -0.000000000000000000 ) ) ;
#5528 = EDGE_CURVE ( 'NONE', #4948, #1037, #7141, .T. ) ;
#5529 = FACE_OUTER_BOUND ( 'NONE', #4541, .T. ) ;
#5530 = DIRECTION ( 'NONE',  ( 1.000000000000000000, 0.000000000000000000, 0.000000000000000000 ) ) ;
#5531 =( LENGTH_UNIT ( ) NAMED_UNIT ( * ) SI_UNIT ( .MILLI., .METRE. ) );
#5532 = VECTOR ( 'NONE', #7839, 1000.000000000000000 ) ;
#5533 = VERTEX_POINT ( 'NONE', #4731 ) ;
#5534 = VERTEX_POINT ( 'NONE', #5284 ) ;
#5535 = VECTOR ( 'NONE', #2067, 1000.000000000000114 ) ;
#5536 = ORIENTED_EDGE ( 'NONE', *, *, #4371, .T. ) ;
#5537 = CARTESIAN_POINT ( 'NONE',  ( -39.99999999999999289, -39.99999999999999289, 10.00000000000000000 ) ) ;
#5538 = CARTESIAN_POINT ( 'NONE',  ( -30.00000000000000355, -29.99999999999999289, 10.00000000000000000 ) ) ;
#5539 = DIRECTION ( 'NONE',  ( -1.000000000000000000, 8.881784197001252323E-16, 0.000000000000000000 ) ) ;
#5540 = UNCERTAINTY_MEASURE_WITH_UNIT (LENGTH_MEASURE( 1.000000000000000082E-05 ), #2304, 'distance_accuracy_value', 'NONE');
#5541 = ORIENTED_EDGE ( 'NONE', *, *, #6599, .T. ) ;
#5542 = LINE ( 'NONE', #5467, #7652 ) ;
#5543 = ADVANCED_FACE ( 'NONE', ( #2124, #5936 ), #4657, .F. ) ;
#5544 = ORIENTED_EDGE ( 'NONE', *, *, #1519, .F. ) ;
#5545 = ORIENTED_EDGE ( 'NONE', *, *, #3347, .F. ) ;
#5546 = AXIS2_PLACEMENT_3D ( 'NONE', #3670, #2332, #4165 ) ;
#5547 = FACE_OUTER_BOUND ( 'NONE', #2549, .T. ) ;
#5548 = CARTESIAN_POINT ( 'NONE',  ( -41.93162583688302902, 82.60437000624546044, -0.1928873818977043519 ) ) ;
#5549 = VECTOR ( 'NONE', #5645, 1000.000000000000000 ) ;
#5550 = PRESENTATION_STYLE_ASSIGNMENT (( #4391 ) ) ;
#5551 = CIRCLE ( 'NONE', #2504, 2.099999999999999645 ) ;
#5552 = FACE_OUTER_BOUND ( 'NONE', #6054, .T. ) ;
#5553 = EDGE_CURVE ( 'NONE', #6876, #7471, #2787, .T. ) ;
#5554 = AXIS2_PLACEMENT_3D ( 'NONE', #7991, #3644, #2851 ) ;
#5555 = ORIENTED_EDGE ( 'NONE', *, *, #84, .T. ) ;
#5556 = VERTEX_POINT ( 'NONE', #4072 ) ;
#5557 = CARTESIAN_POINT ( 'NONE',  ( 2.000000000000000000, -1.329782007511004727, 0.7677500000000014868 ) ) ;
#5558 = DIRECTION ( 'NONE',  ( -0.000000000000000000, -0.000000000000000000, 1.000000000000000000 ) ) ;
#5559 = LINE ( 'NONE', #1914, #114 ) ;
#5560 = CIRCLE ( 'NONE', #6477, 1.610000000000000098 ) ;
#5561 = CARTESIAN_POINT ( 'NONE',  ( 32.65000000000000568, -29.99999999999997868, 10.00000000000000000 ) ) ;
#5562 = AXIS2_PLACEMENT_3D ( 'NONE', #7800, #3526, #316 ) ;
#5563 = DIRECTION ( 'NONE',  ( -1.000000000000000000, 0.000000000000000000, 0.000000000000000000 ) ) ;
#5564 = AXIS2_PLACEMENT_3D ( 'NONE', #233, #7182, #899 ) ;
#5565 = DIRECTION ( 'NONE',  ( -1.000000000000000000, 0.000000000000000000, 0.000000000000000000 ) ) ;
#5566 = ADVANCED_FACE ( 'NONE', ( #3456 ), #5979, .F. ) ;
#5567 = VERTEX_POINT ( 'NONE', #2050 ) ;
#5568 = EDGE_LOOP ( 'NONE', ( #3497, #349, #4217 ) ) ;
#5569 = AXIS2_PLACEMENT_3D ( 'NONE', #28, #651, #1952 ) ;
#5570 = CARTESIAN_POINT ( 'NONE',  ( -4.000000000000000000, 0.7862748000878179155, -2.665527722372434738 ) ) ;
#5571 = CIRCLE ( 'NONE', #7553, 2.750000000000000000 ) ;
#5572 = FACE_BOUND ( 'NONE', #1530, .T. ) ;
#5573 = FACE_OUTER_BOUND ( 'NONE', #4055, .T. ) ;
#5574 = CARTESIAN_POINT ( 'NONE',  ( 0.1499999999999973577, 0.000000000000000000, 2.600000000000000089 ) ) ;
#5575 = CARTESIAN_POINT ( 'NONE',  ( -2.248460506220263166, 6.633023922978178888, 8.003471350439957277 ) ) ;
#5576 = CARTESIAN_POINT ( 'NONE',  ( 50.00000000000003553, 85.00000000000012790, 2.399999999999971489 ) ) ;
#5577 = CIRCLE ( 'NONE', #8078, 2.149999999999995470 ) ;
#5578 = ORIENTED_EDGE ( 'NONE', *, *, #6337, .T. ) ;
#5579 = AXIS2_PLACEMENT_3D ( 'NONE', #6855, #4962, #1671 ) ;
#5580 = AXIS2_PLACEMENT_3D ( 'NONE', #3469, #5993, #1226 ) ;
#5581 = AXIS2_PLACEMENT_3D ( 'NONE', #435, #3607, #2939 ) ;
#5582 = EDGE_LOOP ( 'NONE', ( #489, #4166 ) ) ;
#5583 = VERTEX_POINT ( 'NONE', #2326 ) ;
#5584 = ORIENTED_EDGE ( 'NONE', *, *, #2137, .F. ) ;
#5585 = PRODUCT ( 'socket head cap screw_iso_ISO 4762 M3 x 8 - 8N', 'socket head cap screw_iso_ISO 4762 M3 x 8 - 8N', '', ( #6555 ) ) ;
#5586 = LINE ( 'NONE', #7317, #4771 ) ;
#5587 = FACE_OUTER_BOUND ( 'NONE', #7851, .T. ) ;
#5588 = CIRCLE ( 'NONE', #1872, 2.649999999999999467 ) ;
#5589 = DIRECTION ( 'NONE',  ( -1.000000000000000000, 0.000000000000000000, 0.000000000000000000 ) ) ;
#5590 = ORIENTED_EDGE ( 'NONE', *, *, #7692, .F. ) ;
#5591 = FACE_OUTER_BOUND ( 'NONE', #6763, .T. ) ;
#5592 = PRESENTATION_LAYER_ASSIGNMENT (  '', '', ( #3061 ) ) ;
#5593 = VERTEX_POINT ( 'NONE', #6142 ) ;
#5594 = ORIENTED_EDGE ( 'NONE', *, *, #2930, .T. ) ;
#5595 = DIRECTION ( 'NONE',  ( 0.000000000000000000, -0.000000000000000000, -1.000000000000000000 ) ) ;
#5596 = EDGE_CURVE ( 'NONE', #366, #4852, #6180, .T. ) ;
#5597 = FACE_OUTER_BOUND ( 'NONE', #603, .T. ) ;
#5598 = ADVANCED_FACE ( 'NONE', ( #1077 ), #448, .F. ) ;
#5599 = CARTESIAN_POINT ( 'NONE',  ( -31.74999999999995737, 0.000000000000000000, 0.000000000000000000 ) ) ;
#5600 = B_SPLINE_CURVE_WITH_KNOTS ( 'NONE', 3,
 ( #2845, #2176, #2882, #4023 ),
 .UNSPECIFIED., .F., .F.,
 ( 4, 4 ),
 ( 2.380737581608157039E-07, 0.002336974151641575941 ),
 .UNSPECIFIED. ) ;
#5601 = ORIENTED_EDGE ( 'NONE', *, *, #1898, .T. ) ;
#5602 = EDGE_LOOP ( 'NONE', ( #2934, #5541, #3373, #5544 ) ) ;
#5603 = CARTESIAN_POINT ( 'NONE',  ( 0.000000000000000000, 0.000000000000000000, 0.000000000000000000 ) ) ;
#5604 = LINE ( 'NONE', #4308, #7140 ) ;
#5605 = CARTESIAN_POINT ( 'NONE',  ( 0.1499999999999973577, 0.000000000000000000, 0.000000000000000000 ) ) ;
#5606 = DIRECTION ( 'NONE',  ( 1.412205397084881070E-17, -2.775557561562891967E-17, -1.000000000000000000 ) ) ;
#5607 = DIRECTION ( 'NONE',  ( -0.000000000000000000, -0.000000000000000000, 1.000000000000000000 ) ) ;
#5608 = DIRECTION ( 'NONE',  ( 0.000000000000000000, 1.000000000000000000, -1.224646799147353207E-16 ) ) ;
#5609 = CIRCLE ( 'NONE', #6405, 4.999999999999993783 ) ;
#5610 = VERTEX_POINT ( 'NONE', #4908 ) ;
#5611 = EDGE_CURVE ( 'NONE', #4563, #5767, #3431, .T. ) ;
#5612 = ORIENTED_EDGE ( 'NONE', *, *, #7077, .T. ) ;
#5613 = CARTESIAN_POINT ( 'NONE',  ( 2.500000000000002220, -2.357898499370430834, 3.469446951953614189E-15 ) ) ;
#5614 = DIRECTION ( 'NONE',  ( 1.000000000000000000, 1.502586498047605218E-16, -1.412205397084881070E-17 ) ) ;
#5615 = DIRECTION ( 'NONE',  ( 1.000000000000000000, 0.000000000000000000, 0.000000000000000000 ) ) ;
#5616 = CARTESIAN_POINT ( 'NONE',  ( 58.00000000000000000, 8.000000000000000000, -8.000000000000000000 ) ) ;
#5617 = CIRCLE ( 'NONE', #2035, 10.00000000000000000 ) ;
#5618 = EDGE_CURVE ( 'NONE', #5289, #7441, #4086, .T. ) ;
#5619 = CARTESIAN_POINT ( 'NONE',  ( 30.00000000000001066, -29.99999999999997868, 4.599999999999997868 ) ) ;
#5620 = CYLINDRICAL_SURFACE ( 'NONE', #495, 3.500000000000000000 ) ;
#5621 = CONTEXT_DEPENDENT_SHAPE_REPRESENTATION ( #64, #6240 ) ;
#5622 = ORIENTED_EDGE ( 'NONE', *, *, #2494, .T. ) ;
#5623 = EDGE_LOOP ( 'NONE', ( #930, #2231, #3664 ) ) ;
#5624 = ORIENTED_EDGE ( 'NONE', *, *, #1343, .F. ) ;
#5625 = VERTEX_POINT ( 'NONE', #3492 ) ;
#5626 = CARTESIAN_POINT ( 'NONE',  ( -42.00000000000000000, 84.76402542465484657, 2.400000000000002576 ) ) ;
#5627 = DIRECTION ( 'NONE',  ( 0.000000000000000000, 0.000000000000000000, -1.000000000000000000 ) ) ;
#5628 = LINE ( 'NONE', #497, #6078 ) ;
#5629 = ORIENTED_EDGE ( 'NONE', *, *, #2608, .F. ) ;
#5630 = CARTESIAN_POINT ( 'NONE',  ( 50.00000000000003553, 85.00000000000012790, 2.399999999999971489 ) ) ;
#5631 = ORIENTED_EDGE ( 'NONE', *, *, #7656, .T. ) ;
#5632 = ORIENTED_EDGE ( 'NONE', *, *, #4682, .T. ) ;
#5633 = EDGE_CURVE ( 'NONE', #3736, #5610, #319, .T. ) ;
#5634 = STYLED_ITEM ( 'NONE', ( #834 ), #5769 ) ;
#5635 = EDGE_CURVE ( 'NONE', #5411, #6584, #2362, .T. ) ;
#5636 = DIRECTION ( 'NONE',  ( 0.000000000000000000, 0.000000000000000000, 1.000000000000000000 ) ) ;
#5637 = EDGE_CURVE ( 'NONE', #7949, #741, #3026, .T. ) ;
#5638 = CARTESIAN_POINT ( 'NONE',  ( -41.95061225082201162, 82.96247244883227268, -1.274660781186474745 ) ) ;
#5639 = DIRECTION ( 'NONE',  ( 0.000000000000000000, -9.783878858594330870E-16, -1.000000000000000000 ) ) ;
#5640 = PRODUCT_DEFINITION_FORMATION_WITH_SPECIFIED_SOURCE ( 'ANY', '', #8089, .NOT_KNOWN. ) ;
#5641 = DIRECTION ( 'NONE',  ( 1.000000000000000000, 0.000000000000000000, 0.000000000000000000 ) ) ;
#5642 = VERTEX_POINT ( 'NONE', #2949 ) ;
#5643 = EDGE_LOOP ( 'NONE', ( #4373, #5719 ) ) ;
#5644 = CIRCLE ( 'NONE', #3642, 2.149999999999992362 ) ;
#5645 = DIRECTION ( 'NONE',  ( 0.000000000000000000, -1.000000000000000000, 0.000000000000000000 ) ) ;
#5646 = CARTESIAN_POINT ( 'NONE',  ( 0.000000000000000000, 0.000000000000000000, 18.00000000000000355 ) ) ;
#5647 = CARTESIAN_POINT ( 'NONE',  ( 0.000000000000000000, 0.000000000000000000, 0.000000000000000000 ) ) ;
#5648 = DIRECTION ( 'NONE',  ( -1.000000000000000000, 0.000000000000000000, 0.000000000000000000 ) ) ;
#5649 = CARTESIAN_POINT ( 'NONE',  ( 0.000000000000000000, 0.000000000000000000, 3.469446951953614189E-15 ) ) ;
#5650 = CARTESIAN_POINT ( 'NONE',  ( 0.000000000000000000, 37.49999999999999289, 0.000000000000000000 ) ) ;
#5651 = EDGE_CURVE ( 'NONE', #2831, #6759, #6875, .T. ) ;
#5652 = EDGE_LOOP ( 'NONE', ( #1459, #3964, #1699 ) ) ;
#5653 = CARTESIAN_POINT ( 'NONE',  ( -2.681483223904239210, 3.070647092368425923, 2.403443949632593102E-15 ) ) ;
#5654 = CARTESIAN_POINT ( 'NONE',  ( 0.000000000000000000, 1.178949249685212086, -2.042000000000002036 ) ) ;
#5655 = DIRECTION ( 'NONE',  ( -0.000000000000000000, -0.000000000000000000, 1.000000000000000000 ) ) ;
#5656 = CARTESIAN_POINT ( 'NONE',  ( -4.000000000000000000, -1.549102112939103160, -0.1578953385959410982 ) ) ;
#5657 = DIRECTION ( 'NONE',  ( 0.000000000000000000, 1.000000000000000000, -1.222984857324291014E-15 ) ) ;
#5658 = CARTESIAN_POINT ( 'NONE',  ( 49.94817596271298044, 87.27669880683390602, 0.7754554817173049397 ) ) ;
#5659 = ORIENTED_EDGE ( 'NONE', *, *, #2966, .T. ) ;
#5660 = EDGE_CURVE ( 'NONE', #4900, #5386, #4796, .T. ) ;
#5661 = EDGE_CURVE ( 'NONE', #1110, #8109, #4361, .T. ) ;
#5662 = EDGE_LOOP ( 'NONE', ( #5039, #5594, #1687 ) ) ;
#5663 = DIRECTION ( 'NONE',  ( 0.000000000000000000, -0.000000000000000000, 1.000000000000000000 ) ) ;
#5664 = VERTEX_POINT ( 'NONE', #7968 ) ;
#5665 = ORIENTED_EDGE ( 'NONE', *, *, #3006, .F. ) ;
#5666 = CIRCLE ( 'NONE', #5262, 2.700000000000000622 ) ;
#5667 = DIRECTION ( 'NONE',  ( 0.000000000000000000, -0.000000000000000000, -1.000000000000000000 ) ) ;
#5668 = DIRECTION ( 'NONE',  ( 1.000000000000000000, 0.000000000000000000, 0.000000000000000000 ) ) ;
#5669 = DIRECTION ( 'NONE',  ( 0.000000000000000000, 0.000000000000000000, 1.000000000000000000 ) ) ;
#5670 = EDGE_LOOP ( 'NONE', ( #2954, #4866, #5164 ) ) ;
#5671 = CARTESIAN_POINT ( 'NONE',  ( 49.96363327394941933, 83.09135878423523991, 1.463402463581969348 ) ) ;
#5672 = VECTOR ( 'NONE', #2109, 1000.000000000000000 ) ;
#5673 = VECTOR ( 'NONE', #7007, 1000.000000000000000 ) ;
#5674 = EDGE_LOOP ( 'NONE', ( #3091, #4405, #6155, #6801 ) ) ;
#5675 = ORIENTED_EDGE ( 'NONE', *, *, #1369, .F. ) ;
#5676 = B_SPLINE_CURVE_WITH_KNOTS ( 'NONE', 3,
 ( #5796, #5723, #2637, #3231, #8190, #5145, #7661, #2059, #4514, #5108, #7041, #6957, #89, #1310, #5186, #7625, #3967, #7705, #2517, #750, #3301, #4467, #4553, #7079, #798, #3813, #5837, #1944 ),
 .UNSPECIFIED., .F., .F.,
 ( 4, 2, 2, 2, 2, 2, 2, 2, 2, 2, 2, 2, 2, 4 ),
 ( 0.000000000000000000, 0.0007633435184945318005, 0.001526687036989063601, 0.001908358796236322291, 0.002290030555483581198, 0.002671702314730840105, 0.003053374073978099446, 0.003435045833225358353, 0.003816717592472616827, 0.004198389351719875734, 0.004580061110967133774, 0.004961732870214391813, 0.005343404629461648986, 0.006106748147956165065 ),
 .UNSPECIFIED. ) ;
#5677 = DIRECTION ( 'NONE',  ( -1.000000000000000000, -0.000000000000000000, -0.000000000000000000 ) ) ;
#5678 = CARTESIAN_POINT ( 'NONE',  ( 2.000000000000000000, -0.8865213383406685965, 1.535500000000000531 ) ) ;
#5679 = LINE ( 'NONE', #3268, #5281 ) ;
#5680 = DIRECTION ( 'NONE',  ( -0.000000000000000000, -0.000000000000000000, -1.000000000000000000 ) ) ;
#5681 = CARTESIAN_POINT ( 'NONE',  ( 2.650000000000010125, 0.000000000000000000, 5.400000000000002132 ) ) ;
#5682 = ORIENTED_EDGE ( 'NONE', *, *, #6326, .F. ) ;
#5683 = EDGE_LOOP ( 'NONE', ( #3795, #2333, #7809 ) ) ;
#5684 = CARTESIAN_POINT ( 'NONE',  ( 4.000000000000003553, -0.7779732554280840429, -0.03354435108168055818 ) ) ;
#5685 = CARTESIAN_POINT ( 'NONE',  ( 34.99999999999997868, 30.00000000000001421, 10.00000000000000000 ) ) ;
#5686 = CARTESIAN_POINT ( 'NONE',  ( 0.000000000000000000, 0.000000000000000000, 4.000000000000000000 ) ) ;
#5687 = CARTESIAN_POINT ( 'NONE',  ( 3.000000000000000000, 0.000000000000000000, -1.600000000000000311 ) ) ;
#5688 = DIRECTION ( 'NONE',  ( 0.000000000000000000, 0.000000000000000000, -1.000000000000000000 ) ) ;
#5689 = EDGE_CURVE ( 'NONE', #6902, #4877, #3304, .T. ) ;
#5690 = CARTESIAN_POINT ( 'NONE',  ( 1.214306433183764966E-14, 4.618802153517020059, 0.000000000000000000 ) ) ;
#5691 = VECTOR ( 'NONE', #1626, 1000.000000000000000 ) ;
#5692 = ORIENTED_EDGE ( 'NONE', *, *, #3629, .F. ) ;
#5693 = DIRECTION ( 'NONE',  ( 0.000000000000000000, 0.000000000000000000, 1.000000000000000000 ) ) ;
#5694 = CARTESIAN_POINT ( 'NONE',  ( 0.000000000000000000, 0.000000000000000000, -0.3080913168122707546 ) ) ;
#5695 = CARTESIAN_POINT ( 'NONE',  ( 30.00000000000001066, -29.99999999999997868, 1.734723475976807094E-15 ) ) ;
#5696 = VECTOR ( 'NONE', #3823, 1000.000000000000000 ) ;
#5697 = FACE_OUTER_BOUND ( 'NONE', #7840, .T. ) ;
#5698 = ADVANCED_FACE ( 'NONE', ( #1029 ), #3576, .T. ) ;
#5699 = CARTESIAN_POINT ( 'NONE',  ( 49.94811673897446269, 87.27799541866322386, -0.7717081223119550693 ) ) ;
#5700 = EDGE_CURVE ( 'NONE', #3778, #3851, #4362, .T. ) ;
#5701 = EDGE_LOOP ( 'NONE', ( #7358, #7864, #5885, #389 ) ) ;
#5702 = EDGE_CURVE ( 'NONE', #1678, #135, #538, .T. ) ;
#5703 = EDGE_CURVE ( 'NONE', #3085, #5556, #1569, .T. ) ;
#5704 = AXIS2_PLACEMENT_3D ( 'NONE', #5992, #209, #1438 ) ;
#5705 = ORIENTED_EDGE ( 'NONE', *, *, #2432, .T. ) ;
#5706 = LINE ( 'NONE', #3125, #6370 ) ;
#5707 = ORIENTED_EDGE ( 'NONE', *, *, #7250, .F. ) ;
#5708 = ORIENTED_EDGE ( 'NONE', *, *, #8123, .T. ) ;
#5709 = AXIS2_PLACEMENT_3D ( 'NONE', #5520, #1199, #6265 ) ;
#5710 = PLANE ( 'NONE',  #1193 ) ;
#5711 = CARTESIAN_POINT ( 'NONE',  ( 29.99999999999997868, 30.00000000000001421, 4.599999999999997868 ) ) ;
#5712 = LINE ( 'NONE', #8, #7011 ) ;
#5713 = VECTOR ( 'NONE', #1179, 1000.000000000000000 ) ;
#5714 = CARTESIAN_POINT ( 'NONE',  ( -13.92819135861234159, 20.19450253318626309, 4.999999999999993783 ) ) ;
#5715 = VECTOR ( 'NONE', #7362, 1000.000000000000000 ) ;
#5716 = ORIENTED_EDGE ( 'NONE', *, *, #5300, .T. ) ;
#5717 = DIRECTION ( 'NONE',  ( 1.412205397084881070E-17, -2.775557561562891967E-17, -1.000000000000000000 ) ) ;
#5718 =( REPRESENTATION_RELATIONSHIP ('NONE','NONE', #3916, #3059 ) REPRESENTATION_RELATIONSHIP_WITH_TRANSFORMATION ( #2364 )SHAPE_REPRESENTATION_RELATIONSHIP( ) );
#5719 = ORIENTED_EDGE ( 'NONE', *, *, #1117, .T. ) ;
#5720 = ORIENTED_EDGE ( 'NONE', *, *, #4751, .T. ) ;
#5721 = VECTOR ( 'NONE', #5376, 1000.000000000000114 ) ;
#5722 = FACE_BOUND ( 'NONE', #1712, .T. ) ;
#5723 = CARTESIAN_POINT ( 'NONE',  ( 41.97224725382100274, 86.54166769553343386, 1.857373340501009107 ) ) ;
#5724 = DIRECTION ( 'NONE',  ( -0.000000000000000000, -0.000000000000000000, 1.000000000000000000 ) ) ;
#5726 = EDGE_CURVE ( 'NONE', #5610, #5411, #3833, .T. ) ;
#5725 =( NAMED_UNIT ( * ) SI_UNIT ( $, .STERADIAN. ) SOLID_ANGLE_UNIT ( ) );
#5727 = PRODUCT_DEFINITION_SHAPE ( 'NONE', 'NONE',  #8221 ) ;
#5728 =( GEOMETRIC_REPRESENTATION_CONTEXT ( 3 ) GLOBAL_UNCERTAINTY_ASSIGNED_CONTEXT ( ( #2881 ) ) GLOBAL_UNIT_ASSIGNED_CONTEXT ( ( #1183, #1816, #3600 ) ) REPRESENTATION_CONTEXT ( 'NONE', 'WORKASPACE' ) );
#5729 = LINE ( 'NONE', #7083, #4255 ) ;
#5730 = VECTOR ( 'NONE', #7862, 1000.000000000000000 ) ;
#5731 = VERTEX_POINT ( 'NONE', #6358 ) ;
#5732 = CARTESIAN_POINT ( 'NONE',  ( 55.00000000000000000, -10.00000000000000000, 13.35000000000001030 ) ) ;
#5733 = DIRECTION ( 'NONE',  ( -1.000000000000000000, -0.000000000000000000, -0.000000000000000000 ) ) ;
#5734 = CARTESIAN_POINT ( 'NONE',  ( -29.99999999999999289, 30.00000000000000711, 4.599999999999997868 ) ) ;
#5735 = CARTESIAN_POINT ( 'NONE',  ( 20.00000000000000355, 0.000000000000000000, 0.000000000000000000 ) ) ;
#5736 = DIRECTION ( 'NONE',  ( -0.000000000000000000, 1.000000000000000000, -0.000000000000000000 ) ) ;
#5737 = DIRECTION ( 'NONE',  ( 0.000000000000000000, 1.000000000000000000, -0.000000000000000000 ) ) ;
#5738 = EDGE_LOOP ( 'NONE', ( #5056, #5516, #2143 ) ) ;
#5739 = DIRECTION ( 'NONE',  ( 0.000000000000000000, 0.000000000000000000, 1.000000000000000000 ) ) ;
#5740 = EDGE_CURVE ( 'NONE', #1216, #3168, #7479, .T. ) ;
#5741 = DIRECTION ( 'NONE',  ( -1.412205397084881070E-17, 2.775557561562891967E-17, 1.000000000000000000 ) ) ;
#5742 = FACE_OUTER_BOUND ( 'NONE', #545, .T. ) ;
#5743 = DIRECTION ( 'NONE',  ( -0.000000000000000000, -1.000000000000000000, -0.000000000000000000 ) ) ;
#5744 = ADVANCED_FACE ( 'NONE', ( #6313 ), #5088, .F. ) ;
#5745 = CARTESIAN_POINT ( 'NONE',  ( 50.00000000000004974, 85.00000000000039790, -2.399999999999999467 ) ) ;
#5746 = EDGE_LOOP ( 'NONE', ( #2106, #5781, #7391, #5060 ) ) ;
#5747 = ORIENTED_EDGE ( 'NONE', *, *, #4321, .T. ) ;
#5748 = PRODUCT_DEFINITION ( 'UNKNOWN', '', #289, #3170 ) ;
#5749 = DIRECTION ( 'NONE',  ( -0.000000000000000000, -1.000000000000000000, -0.000000000000000000 ) ) ;
#5750 = ORIENTED_EDGE ( 'NONE', *, *, #1737, .F. ) ;
#5751 = CIRCLE ( 'NONE', #8115, 2.041999999999999815 ) ;
#5752 = EDGE_LOOP ( 'NONE', ( #4844, #6486, #4, #2055, #7022 ) ) ;
#5753 = DIRECTION ( 'NONE',  ( 0.000000000000000000, -1.000000000000000000, 0.000000000000000000 ) ) ;
#5754 = CARTESIAN_POINT ( 'NONE',  ( 2.000000000000000000, 1.773042676681340968, -2.276824562219559311E-15 ) ) ;
#5755 = LINE ( 'NONE', #6986, #7550 ) ;
#5756 = DIRECTION ( 'NONE',  ( 1.000000000000000000, 1.363075293218191931E-18, 6.123233995736766036E-17 ) ) ;
#5757 = EDGE_LOOP ( 'NONE', ( #4398, #6437, #3955 ) ) ;
#5758 = EDGE_LOOP ( 'NONE', ( #4123, #6130, #1, #5210, #2127 ) ) ;
#5759 = EDGE_CURVE ( 'NONE', #7471, #2461, #615, .T. ) ;
#5760 = VERTEX_POINT ( 'NONE', #36 ) ;
#5761 = EDGE_CURVE ( 'NONE', #7226, #6726, #3810, .T. ) ;
#5762 = CARTESIAN_POINT ( 'NONE',  ( 0.000000000000000000, 37.49999999999999289, 4.000000000000000000 ) ) ;
#5763 = CARTESIAN_POINT ( 'NONE',  ( 41.94437084781012715, 82.83815445687697832, 1.050092974071257235 ) ) ;
#5764 = DIRECTION ( 'NONE',  ( 0.000000000000000000, -1.000000000000000000, 1.103561164596346103E-15 ) ) ;
#5765 =( NAMED_UNIT ( * ) SI_UNIT ( $, .STERADIAN. ) SOLID_ANGLE_UNIT ( ) );
#5766 = ADVANCED_FACE ( 'NONE', ( #1925 ), #1153, .F. ) ;
#5767 = VERTEX_POINT ( 'NONE', #6893 ) ;
#5768 = DIRECTION ( 'NONE',  ( 0.000000000000000000, 0.000000000000000000, 1.000000000000000000 ) ) ;
#5769 = ADVANCED_BREP_SHAPE_REPRESENTATION ( '', ( #1426, #1587 ), #3250 ) ;
#5770 = AXIS2_PLACEMENT_3D ( 'NONE', #165, #4547, #3924 ) ;
#5771 = PLANE ( 'NONE',  #5207 ) ;
#5772 = CYLINDRICAL_SURFACE ( 'NONE', #5008, 2.149999999999995470 ) ;
#5773 = VECTOR ( 'NONE', #8167, 1000.000000000000000 ) ;
#5774 = ORIENTED_EDGE ( 'NONE', *, *, #549, .F. ) ;
#5775 = DIRECTION ( 'NONE',  ( 0.000000000000000000, 0.000000000000000000, 1.000000000000000000 ) ) ;
#5776 = APPLICATION_CONTEXT ( 'automotive_design' ) ;
#5777 = FILL_AREA_STYLE ('',( #3948 ) ) ;
#5778 = CARTESIAN_POINT ( 'NONE',  ( 0.2500000000000002220, 0.000000000000000000, 4.250000000000021316 ) ) ;
#5779 = DIRECTION ( 'NONE',  ( 1.000000000000000000, 0.000000000000000000, 0.000000000000000000 ) ) ;
#5780 = FACE_OUTER_BOUND ( 'NONE', #2077, .T. ) ;
#5781 = ORIENTED_EDGE ( 'NONE', *, *, #8049, .F. ) ;
#5782 = VERTEX_POINT ( 'NONE', #664 ) ;
#5783 = ADVANCED_FACE ( 'NONE', ( #7016 ), #69, .F. ) ;
#5784 = DIRECTION ( 'NONE',  ( -0.000000000000000000, -0.000000000000000000, 1.000000000000000000 ) ) ;
#5785 = EDGE_CURVE ( 'NONE', #3954, #910, #2104, .T. ) ;
#5786 = VERTEX_POINT ( 'NONE', #3162 ) ;
#5787 = ORIENTED_EDGE ( 'NONE', *, *, #4828, .T. ) ;
#5788 = FACE_OUTER_BOUND ( 'NONE', #8187, .T. ) ;
#5789 = LINE ( 'NONE', #2017, #2126 ) ;
#5790 = LINE ( 'NONE', #5217, #8063 ) ;
#5791 = CARTESIAN_POINT ( 'NONE',  ( 2.359758559326825638E-14, 55.01196202519795264, 12.00000000000001776 ) ) ;
#5792 = ORIENTED_EDGE ( 'NONE', *, *, #7733, .T. ) ;
#5793 = VERTEX_POINT ( 'NONE', #2584 ) ;
#5794 = ORIENTED_EDGE ( 'NONE', *, *, #820, .F. ) ;
#5795 = CARTESIAN_POINT ( 'NONE',  ( 0.000000000000000000, 0.000000000000000000, 10.00000000000000000 ) ) ;
#5796 = CARTESIAN_POINT ( 'NONE',  ( 41.97904239022138029, 86.32664991614251448, 2.000000000000043521 ) ) ;
#5797 = CARTESIAN_POINT ( 'NONE',  ( 2.500000000000002220, -1.178949249685215417, 2.042000000000002036 ) ) ;
#5798 = SURFACE_STYLE_USAGE ( .BOTH. , #3815 ) ;
#5799 = ADVANCED_FACE ( 'NONE', ( #5697 ), #3969, .T. ) ;
#5800 = EDGE_CURVE ( 'NONE', #3286, #5533, #6975, .T. ) ;
#5801 = AXIS2_PLACEMENT_3D ( 'NONE', #2191, #4033, #4724 ) ;
#5802 =( LENGTH_UNIT ( ) NAMED_UNIT ( * ) SI_UNIT ( .MILLI., .METRE. ) );
#5803 = DIRECTION ( 'NONE',  ( -0.000000000000000000, -0.000000000000000000, -1.000000000000000000 ) ) ;
#5804 = DIRECTION ( 'NONE',  ( 0.000000000000000000, 0.000000000000000000, 1.000000000000000000 ) ) ;
#5805 = CARTESIAN_POINT ( 'NONE',  ( 4.000000000000000000, 0.000000000000000000, 0.000000000000000000 ) ) ;
#5806 = DIRECTION ( 'NONE',  ( -0.000000000000000000, -0.000000000000000000, -1.000000000000000000 ) ) ;
#5807 = CARTESIAN_POINT ( 'NONE',  ( -3.469446951953613006E-15, 0.000000000000000000, 20.00000000000000355 ) ) ;
#5808 = ORIENTED_EDGE ( 'NONE', *, *, #4128, .F. ) ;
#5809 = FACE_OUTER_BOUND ( 'NONE', #1766, .T. ) ;
#5810 = FILL_AREA_STYLE_COLOUR ( '', #4901 ) ;
#5811 = CARTESIAN_POINT ( 'NONE',  ( 2.500000000000002220, 0.000000000000000000, 0.000000000000000000 ) ) ;
#5812 = CARTESIAN_POINT ( 'NONE',  ( 0.1499999999999973577, 0.000000000000000000, 0.000000000000000000 ) ) ;
#5813 = CARTESIAN_POINT ( 'NONE',  ( 39.83716857408421674, 108.0000000000001137, 0.7510757737844986348 ) ) ;
#5814 = PRESENTATION_LAYER_ASSIGNMENT (  '', '', ( #213 ) ) ;
#5815 = EDGE_CURVE ( 'NONE', #5387, #2626, #1568, .T. ) ;
#5816 = ORIENTED_EDGE ( 'NONE', *, *, #716, .F. ) ;
#5817 = EDGE_LOOP ( 'NONE', ( #502, #1853, #6944, #2428 ) ) ;
#5818 = CARTESIAN_POINT ( 'NONE',  ( 1.270137496355039850E-14, 85.00000000000011369, 5.000000000000046185 ) ) ;
#5819 = ORIENTED_EDGE ( 'NONE', *, *, #706, .F. ) ;
#5820 = AXIS2_PLACEMENT_3D ( 'NONE', #787, #163, #743 ) ;
#5821 = ORIENTED_EDGE ( 'NONE', *, *, #88, .F. ) ;
#5822 = CARTESIAN_POINT ( 'NONE',  ( 3.999999999999999112, 3.500000000000000000, 0.000000000000000000 ) ) ;
#5823 = CARTESIAN_POINT ( 'NONE',  ( 29.55500000000002458, 3.061616997868375746E-16, -2.500000000000000888 ) ) ;
#5824 = PLANE ( 'NONE',  #368 ) ;
#5825 = APPLICATION_PROTOCOL_DEFINITION ( 'draft international standard', 'automotive_design', 1998, #5346 ) ;
#5826 = AXIS2_PLACEMENT_3D ( 'NONE', #628, #6244, #8183 ) ;
#5827 = CIRCLE ( 'NONE', #2762, 4.250000000000000000 ) ;
#5828 = AXIS2_PLACEMENT_3D ( 'NONE', #2186, #2974, #1653 ) ;
#5829 = AXIS2_PLACEMENT_3D ( 'NONE', #6139, #4316, #6843 ) ;
#5830 = ORIENTED_EDGE ( 'NONE', *, *, #5024, .T. ) ;
#5831 = ORIENTED_EDGE ( 'NONE', *, *, #1028, .T. ) ;
#5832 = ORIENTED_EDGE ( 'NONE', *, *, #3836, .F. ) ;
#5833 = CIRCLE ( 'NONE', #3725, 7.000000000000000000 ) ;
#5835 = CARTESIAN_POINT ( 'NONE',  ( 0.000000000000000000, -0.8865213383406685965, 1.535500000000000531 ) ) ;
#5834 = AXIS2_PLACEMENT_3D ( 'NONE', #3865, #7086, #5881 ) ;
#5836 = EDGE_CURVE ( 'NONE', #2969, #1899, #7923, .T. ) ;
#5837 = CARTESIAN_POINT ( 'NONE',  ( 42.00000000000004263, 85.25453321192475187, -2.400000000000038991 ) ) ;
#5838 = CARTESIAN_POINT ( 'NONE',  ( 0.000000000000000000, 1.773042676681340968, -2.276824562219559311E-15 ) ) ;
#5839 = EDGE_CURVE ( 'NONE', #7927, #2250, #4625, .T. ) ;
#5840 = VECTOR ( 'NONE', #3608, 1000.000000000000000 ) ;
#5841 = SURFACE_SIDE_STYLE ('',( #7158 ) ) ;
#5842 = CIRCLE ( 'NONE', #6898, 2.649999999999995914 ) ;
#5843 = VECTOR ( 'NONE', #1365, 1000.000000000000000 ) ;
#5844 = AXIS2_PLACEMENT_3D ( 'NONE', #850, #2620, #6544 ) ;
#5845 = EDGE_CURVE ( 'NONE', #3495, #5254, #1378, .T. ) ;
#5846 = FACE_OUTER_BOUND ( 'NONE', #3184, .T. ) ;
#5847 = AXIS2_PLACEMENT_3D ( 'NONE', #7489, #7527, #1894 ) ;
#5848 = LINE ( 'NONE', #3900, #1197 ) ;
#5849 = TOROIDAL_SURFACE ( 'NONE', #1735, 2.200000000000001066, 0.2000000000000000111 ) ;
#5850 = PLANE ( 'NONE',  #928 ) ;
#5851 = CARTESIAN_POINT ( 'NONE',  ( 55.00000000000000000, 10.00000000000000000, 15.50000000000000355 ) ) ;
#5852 = VERTEX_POINT ( 'NONE', #2041 ) ;
#5853 = DIRECTION ( 'NONE',  ( -1.000000000000000000, 0.000000000000000000, -0.000000000000000000 ) ) ;
#5854 = DIRECTION ( 'NONE',  ( 0.000000000000000000, 0.000000000000000000, 1.000000000000000000 ) ) ;
#5855 = DIRECTION ( 'NONE',  ( 0.000000000000000000, 0.000000000000000000, 1.000000000000000000 ) ) ;
#5856 = DIRECTION ( 'NONE',  ( -0.000000000000000000, -0.000000000000000000, 1.000000000000000000 ) ) ;
#5857 = DIRECTION ( 'NONE',  ( 1.000000000000000000, 0.000000000000000000, 0.000000000000000000 ) ) ;
#5858 = ORIENTED_EDGE ( 'NONE', *, *, #4261, .T. ) ;
#5859 = CARTESIAN_POINT ( 'NONE',  ( 49.96742166427393528, 83.19195211451632588, -1.586024383261910309 ) ) ;
#5860 = EDGE_CURVE ( 'NONE', #4304, #4662, #1849, .T. ) ;
#5861 = EDGE_LOOP ( 'NONE', ( #5223, #4063, #2691, #3137, #4188 ) ) ;
#5862 = VERTEX_POINT ( 'NONE', #6543 ) ;
#5863 = ORIENTED_EDGE ( 'NONE', *, *, #4636, .F. ) ;
#5864 = VERTEX_POINT ( 'NONE', #2008 ) ;
#5865 = FACE_OUTER_BOUND ( 'NONE', #6352, .T. ) ;
#5866 = CARTESIAN_POINT ( 'NONE',  ( 60.00000000000000711, -10.00000000000000000, 60.00000000000000000 ) ) ;
#5867 = CARTESIAN_POINT ( 'NONE',  ( 64.00000000000005684, 101.0119620251984571, 6.303019571339394006E-15 ) ) ;
#5868 = ORIENTED_EDGE ( 'NONE', *, *, #665, .F. ) ;
#5869 = ORIENTED_EDGE ( 'NONE', *, *, #3413, .T. ) ;
#5870 = ORIENTED_EDGE ( 'NONE', *, *, #2301, .T. ) ;
#5871 = CARTESIAN_POINT ( 'NONE',  ( -4.999999999999997335, 6.123233995736758394E-16, 14.60000000000000142 ) ) ;
#5872 = LINE ( 'NONE', #4831, #3056 ) ;
#5873 = CARTESIAN_POINT ( 'NONE',  ( 60.00000000000000711, 10.00000000000000000, 19.99999999999998224 ) ) ;
#5874 = AXIS2_PLACEMENT_3D ( 'NONE', #7202, #7328, #2720 ) ;
#5875 =( NAMED_UNIT ( * ) PLANE_ANGLE_UNIT ( ) SI_UNIT ( $, .RADIAN. ) );
#5876 = EDGE_CURVE ( 'NONE', #7622, #2701, #813, .T. ) ;
#5877 = ADVANCED_FACE ( 'NONE', ( #2661 ), #2725, .T. ) ;
#5878 = EDGE_CURVE ( 'NONE', #3946, #7927, #7682, .T. ) ;
#5879 = DIRECTION ( 'NONE',  ( 1.000000000000000000, 0.000000000000000000, 0.000000000000000000 ) ) ;
#5880 = CYLINDRICAL_SURFACE ( 'NONE', #5055, 4.250000000000000000 ) ;
#5881 = DIRECTION ( 'NONE',  ( 0.000000000000000000, 1.224646799147353207E-16, 1.000000000000000000 ) ) ;
#5882 = DIRECTION ( 'NONE',  ( 0.000000000000000000, 0.000000000000000000, -1.000000000000000000 ) ) ;
#5883 = COLOUR_RGB ( '', 0.66274510, 0.83137255, 0.94901961) ;
#5884 = CYLINDRICAL_SURFACE ( 'NONE', #1628, 2.149999999999995470 ) ;
#5885 = ORIENTED_EDGE ( 'NONE', *, *, #6264, .T. ) ;
#5886 = FACE_BOUND ( 'NONE', #1657, .T. ) ;
#5887 = SURFACE_STYLE_FILL_AREA ( #5777 ) ;
#5888 = DIRECTION ( 'NONE',  ( 0.000000000000000000, -1.000000000000000000, 0.000000000000000000 ) ) ;
#5889 =( GEOMETRIC_REPRESENTATION_CONTEXT ( 3 ) GLOBAL_UNCERTAINTY_ASSIGNED_CONTEXT ( ( #1496 ) ) GLOBAL_UNIT_ASSIGNED_CONTEXT ( ( #1674, #416, #1129 ) ) REPRESENTATION_CONTEXT ( 'NONE', 'WORKASPACE' ) );
#5890 = CARTESIAN_POINT ( 'NONE',  ( 20.00000000000000355, 2.210487472460973191E-16, -1.610000000000000098 ) ) ;
#5891 =( LENGTH_UNIT ( ) NAMED_UNIT ( * ) SI_UNIT ( .MILLI., .METRE. ) );
#5892 = CARTESIAN_POINT ( 'NONE',  ( 0.000000000000000000, 0.000000000000000000, 2.600000000000000089 ) ) ;
#5893 = ORIENTED_EDGE ( 'NONE', *, *, #5910, .T. ) ;
#5894 = CARTESIAN_POINT ( 'NONE',  ( 49.98566918070729770, 83.79593159430160654, 2.081985610399850195 ) ) ;
#5895 = UNCERTAINTY_MEASURE_WITH_UNIT (LENGTH_MEASURE( 1.000000000000000082E-05 ), #5909, 'distance_accuracy_value', 'NONE');
#5896 = ORIENTED_EDGE ( 'NONE', *, *, #7808, .F. ) ;
#5897 = ORIENTED_EDGE ( 'NONE', *, *, #7098, .T. ) ;
#5898 = DIRECTION ( 'NONE',  ( 0.000000000000000000, 1.000000000000000000, -1.320393690296331133E-15 ) ) ;
#5899 = CARTESIAN_POINT ( 'NONE',  ( -110.0000000000000711, -3.212021572632693692E-15, 11.99999999999998934 ) ) ;
#5900 = DIRECTION ( 'NONE',  ( 0.000000000000000000, 0.4999999999999991118, -0.8660254037844391517 ) ) ;
#5901 = SHAPE_DEFINITION_REPRESENTATION ( #6827, #3916 ) ;
#5902 = ADVANCED_FACE ( 'NONE', ( #4606 ), #7131, .F. ) ;
#5903 = VERTEX_POINT ( 'NONE', #5890 ) ;
#5904 = ORIENTED_EDGE ( 'NONE', *, *, #4828, .F. ) ;
#5905 = ORIENTED_EDGE ( 'NONE', *, *, #3443, .F. ) ;
#5906 = DIRECTION ( 'NONE',  ( -0.000000000000000000, 0.000000000000000000, 1.000000000000000000 ) ) ;
#5907 = DIRECTION ( 'NONE',  ( 1.000000000000000000, -0.000000000000000000, -0.000000000000000000 ) ) ;
#5908 = CARTESIAN_POINT ( 'NONE',  ( 2.000000000000000000, 1.773042676681340968, -2.276824562219559311E-15 ) ) ;
#5909 =( LENGTH_UNIT ( ) NAMED_UNIT ( * ) SI_UNIT ( .MILLI., .METRE. ) );
#5910 = EDGE_CURVE ( 'NONE', #3614, #3337, #131, .T. ) ;
#5911 = CARTESIAN_POINT ( 'NONE',  ( 2.000000000000000000, 1.329782007511004727, -0.7677500000000019309 ) ) ;
#5912 = LINE ( 'NONE', #6612, #3186 ) ;
#5913 = DIRECTION ( 'NONE',  ( 0.000000000000000000, 0.000000000000000000, -1.000000000000000000 ) ) ;
#5914 = CIRCLE ( 'NONE', #3531, 4.000000000000000000 ) ;
#5915 = CARTESIAN_POINT ( 'NONE',  ( 52.00000000000000711, 8.000000000000000000, 0.000000000000000000 ) ) ;
#5916 = ADVANCED_FACE ( 'NONE', ( #6509 ), #2639, .T. ) ;
#5917 = CARTESIAN_POINT ( 'NONE',  ( -2.000000000000022649, -3.464101615137742396, 0.000000000000000000 ) ) ;
#5918 = LINE ( 'NONE', #5996, #6658 ) ;
#5919 = AXIS2_PLACEMENT_3D ( 'NONE', #2007, #5272, #1410 ) ;
#5920 = EDGE_LOOP ( 'NONE', ( #7770, #3461, #3215 ) ) ;
#5921 = CARTESIAN_POINT ( 'NONE',  ( 2.500000000000002220, 0.000000000000000000, 0.000000000000000000 ) ) ;
#5922 = CARTESIAN_POINT ( 'NONE',  ( 2.678494666091051801, 3.072372537026354156, -2.665789719053470730 ) ) ;
#5923 = FACE_OUTER_BOUND ( 'NONE', #3798, .T. ) ;
#5924 = CARTESIAN_POINT ( 'NONE',  ( 2.000000000000000000, 0.8865213383406687075, -1.535500000000000975 ) ) ;
#5925 = SURFACE_STYLE_USAGE ( .BOTH. , #1379 ) ;
#5926 = CARTESIAN_POINT ( 'NONE',  ( 2.500000000000002220, 2.357898499370434386, -3.469446951953614189E-15 ) ) ;
#5927 = ORIENTED_EDGE ( 'NONE', *, *, #7157, .F. ) ;
#5928 = B_SPLINE_CURVE_WITH_KNOTS ( 'NONE', 3,
 ( #969, #3427, #2214, #5917 ),
 .UNSPECIFIED., .F., .F.,
 ( 4, 4 ),
 ( 2.380737582494095533E-07, 0.002336974151641604998 ),
 .UNSPECIFIED. ) ;
#5929 = CARTESIAN_POINT ( 'NONE',  ( 2.000000000000000000, -0.8865213383406690406, 1.535500000000000975 ) ) ;
#5930 = ORIENTED_EDGE ( 'NONE', *, *, #6816, .T. ) ;
#5931 = ORIENTED_EDGE ( 'NONE', *, *, #3204, .T. ) ;
#5932 = CIRCLE ( 'NONE', #4487, 3.500000000000000000 ) ;
#5933 = ORIENTED_EDGE ( 'NONE', *, *, #5523, .F. ) ;
#5934 = EDGE_CURVE ( 'NONE', #6841, #3736, #6578, .T. ) ;
#5935 = AXIS2_PLACEMENT_3D ( 'NONE', #6001, #2849, #4137 ) ;
#5936 = FACE_OUTER_BOUND ( 'NONE', #4620, .T. ) ;
#5937 = ADVANCED_FACE ( 'NONE', ( #7174 ), #1033, .T. ) ;
#5938 = DIRECTION ( 'NONE',  ( 0.000000000000000000, 0.000000000000000000, 1.000000000000000000 ) ) ;
#5939 = EDGE_CURVE ( 'NONE', #973, #3705, #7721, .T. ) ;
#5940 = AXIS2_PLACEMENT_3D ( 'NONE', #1279, #6963, #2481 ) ;
#5941 = ORIENTED_EDGE ( 'NONE', *, *, #4024, .F. ) ;
#5942 = ORIENTED_EDGE ( 'NONE', *, *, #3613, .F. ) ;
#5943 = ORIENTED_EDGE ( 'NONE', *, *, #33, .F. ) ;
#5944 = DIRECTION ( 'NONE',  ( -1.000000000000000000, 0.000000000000000000, 0.000000000000000000 ) ) ;
#5945 = DIRECTION ( 'NONE',  ( 1.000000000000000000, 0.000000000000000000, 0.000000000000000000 ) ) ;
#5946 = FACE_OUTER_BOUND ( 'NONE', #6020, .T. ) ;
#5947 = CLOSED_SHELL ( 'NONE', ( #4780, #6863, #7593, #438, #2276, #2365, #6785, #1675, #5466, #6478, #4213, #2413, #1953, #5185, #2780, #5598, #4938, #5221, #3263, #6645, #8027, #7588, #4004, #6707, #7761, #594, #7299 ) ) ;
#5948 = AXIS2_PLACEMENT_3D ( 'NONE', #6281, #6946, #5050 ) ;
#5949 = FILL_AREA_STYLE_COLOUR ( '', #5240 ) ;
#5950 = PRESENTATION_LAYER_ASSIGNMENT (  '', '', ( #1324 ) ) ;
#5951 = AXIS2_PLACEMENT_3D ( 'NONE', #567, #5079, #6213 ) ;
#5952 = EDGE_CURVE ( 'NONE', #1216, #452, #849, .T. ) ;
#5953 = DIRECTION ( 'NONE',  ( -1.000000000000000000, 0.000000000000000000, 0.000000000000000000 ) ) ;
#5954 = DIRECTION ( 'NONE',  ( 0.000000000000000000, -1.000000000000000000, 1.287488025362403787E-15 ) ) ;
#5955 = AXIS2_PLACEMENT_3D ( 'NONE', #7507, #4897, #3112 ) ;
#5956 = PRESENTATION_STYLE_ASSIGNMENT (( #335 ) ) ;
#5957 = CARTESIAN_POINT ( 'NONE',  ( 0.000000000000000000, 0.8865213383406685965, -1.535500000000000753 ) ) ;
#5958 = AXIS2_PLACEMENT_3D ( 'NONE', #7907, #5437, #890 ) ;
#5959 = CARTESIAN_POINT ( 'NONE',  ( 55.00000000000000000, -10.00000000000000000, 17.64999999999999503 ) ) ;
#5960 = ORIENTED_EDGE ( 'NONE', *, *, #4204, .T. ) ;
#5961 = PLANE ( 'NONE',  #3921 ) ;
#5962 = VECTOR ( 'NONE', #3257, 1000.000000000000000 ) ;
#5963 = FACE_BOUND ( 'NONE', #7100, .T. ) ;
#5964 = CARTESIAN_POINT ( 'NONE',  ( 1.300000000000000044, -1.478016689125442706, 1.843143693225357538E-15 ) ) ;
#5965 = CARTESIAN_POINT ( 'NONE',  ( 2.000000000000000000, 1.773042676681340968, -2.276824562219559311E-15 ) ) ;
#5966 = DIRECTION ( 'NONE',  ( -0.000000000000000000, -0.000000000000000000, 1.000000000000000000 ) ) ;
#5967 = DIRECTION ( 'NONE',  ( 1.000000000000000000, 0.000000000000000000, 0.000000000000000000 ) ) ;
#5968 = DIRECTION ( 'NONE',  ( -0.000000000000000000, -0.000000000000000000, -1.000000000000000000 ) ) ;
#5969 = EDGE_LOOP ( 'NONE', ( #4548, #6664, #1498, #730 ) ) ;
#5970 = CARTESIAN_POINT ( 'NONE',  ( -59.99999999999999289, 85.00000000000045475, -2.399999999999999467 ) ) ;
#5971 = ORIENTED_EDGE ( 'NONE', *, *, #5939, .T. ) ;
#5972 = EDGE_CURVE ( 'NONE', #6551, #4877, #2147, .T. ) ;
#5973 = ORIENTED_EDGE ( 'NONE', *, *, #1072, .F. ) ;
#5974 = CIRCLE ( 'NONE', #4396, 4.999999999999993783 ) ;
#5975 = CARTESIAN_POINT ( 'NONE',  ( 2.500000000000002220, 1.178949249685218970, 2.041999999999998483 ) ) ;
#5976 = EDGE_CURVE ( 'NONE', #5372, #314, #4534, .T. ) ;
#5977 = LINE ( 'NONE', #1702, #5177 ) ;
#5978 = LINE ( 'NONE', #7881, #4671 ) ;
#5979 = PLANE ( 'NONE',  #6075 ) ;
#5980 = CARTESIAN_POINT ( 'NONE',  ( 1.300000000000000044, -0.7390083445627200209, 1.280000000000001137 ) ) ;
#5981 = SHAPE_DEFINITION_REPRESENTATION ( #5134, #499 ) ;
#5982 = ORIENTED_EDGE ( 'NONE', *, *, #7308, .F. ) ;
#5983 = ORIENTED_EDGE ( 'NONE', *, *, #7948, .T. ) ;
#5984 = ORIENTED_EDGE ( 'NONE', *, *, #3166, .F. ) ;
#5985 = CARTESIAN_POINT ( 'NONE',  ( 0.1999999999999987899, 0.000000000000000000, 0.000000000000000000 ) ) ;
#5986 = CARTESIAN_POINT ( 'NONE',  ( 5.946271935299904499, -3.700516488397892712, 8.024501004382219804 ) ) ;
#5987 = DIRECTION ( 'NONE',  ( -1.000000000000000000, -0.000000000000000000, -0.000000000000000000 ) ) ;
#5988 = CIRCLE ( 'NONE', #7059, 2.041999999999999815 ) ;
#5989 = EDGE_CURVE ( 'NONE', #5664, #973, #734, .T. ) ;
#5990 = ADVANCED_FACE ( 'NONE', ( #2619 ), #772, .F. ) ;
#5991 = AXIS2_PLACEMENT_3D ( 'NONE', #3511, #1646, #4710 ) ;
#5992 = CARTESIAN_POINT ( 'NONE',  ( 19.61000000000001720, 0.000000000000000000, 0.000000000000000000 ) ) ;
#5993 = DIRECTION ( 'NONE',  ( -0.000000000000000000, -0.000000000000000000, 1.000000000000000000 ) ) ;
#5994 = EDGE_CURVE ( 'NONE', #6062, #1727, #1613, .T. ) ;
#5995 = CARTESIAN_POINT ( 'NONE',  ( -3.000000000000000888, 45.09008114612887397, 4.000000000000000000 ) ) ;
#5996 = CARTESIAN_POINT ( 'NONE',  ( -31.74999999999995737, 4.286263797015736595E-16, -3.500000000000000000 ) ) ;
#5997 = FACE_BOUND ( 'NONE', #5288, .T. ) ;
#5998 = VERTEX_POINT ( 'NONE', #6626 ) ;
#5999 = ORIENTED_EDGE ( 'NONE', *, *, #1469, .F. ) ;
#6000 = FACE_OUTER_BOUND ( 'NONE', #1213, .T. ) ;
#6001 = CARTESIAN_POINT ( 'NONE',  ( -30.00000000000000355, -29.99999999999999289, 4.599999999999997868 ) ) ;
#6002 = DIRECTION ( 'NONE',  ( -1.000000000000000000, -0.000000000000000000, -0.000000000000000000 ) ) ;
#6003 = CARTESIAN_POINT ( 'NONE',  ( -41.94112359463809270, 87.22431328320553234, -0.9366119428082910758 ) ) ;
#6004 = CYLINDRICAL_SURFACE ( 'NONE', #7807, 721.2499999999977263 ) ;
#6005 = CARTESIAN_POINT ( 'NONE',  ( 24.00000000000000000, 0.000000000000000000, 0.000000000000000000 ) ) ;
#6006 =( GEOMETRIC_REPRESENTATION_CONTEXT ( 3 ) GLOBAL_UNCERTAINTY_ASSIGNED_CONTEXT ( ( #459 ) ) GLOBAL_UNIT_ASSIGNED_CONTEXT ( ( #722, #1360, #5725 ) ) REPRESENTATION_CONTEXT ( 'NONE', 'WORKASPACE' ) );
#6007 = CARTESIAN_POINT ( 'NONE',  ( 1.300000000000000044, -1.478016689125442706, 1.843143693225357538E-15 ) ) ;
#6008 =( REPRESENTATION_RELATIONSHIP ('NONE','NONE', #3916, #7870 ) REPRESENTATION_RELATIONSHIP_WITH_TRANSFORMATION ( #6770 )SHAPE_REPRESENTATION_RELATIONSHIP( ) );
#6009 = EDGE_LOOP ( 'NONE', ( #5325, #507, #4509, #5578, #8048 ) ) ;
#6010 = LINE ( 'NONE', #5929, #4725 ) ;
#6011 = ORIENTED_EDGE ( 'NONE', *, *, #4925, .F. ) ;
#6012 = VERTEX_POINT ( 'NONE', #265 ) ;
#6013 = LINE ( 'NONE', #7221, #4504 ) ;
#6014 = CARTESIAN_POINT ( 'NONE',  ( 4.000000000000004441, 0.7862748000878159171, -2.665527722372431629 ) ) ;
#6015 = CARTESIAN_POINT ( 'NONE',  ( 52.00000000000000711, -8.000000000000000000, 0.000000000000000000 ) ) ;
#6016 = CARTESIAN_POINT ( 'NONE',  ( -5.944181862675879557, 3.703975565927438041, 8.024483585023222787 ) ) ;
#6017 = DIRECTION ( 'NONE',  ( -1.000000000000000000, -0.000000000000000000, -0.000000000000000000 ) ) ;
#6018 = APPLICATION_PROTOCOL_DEFINITION ( 'draft international standard', 'automotive_design', 1998, #3818 ) ;
#6019 = PRODUCT_DEFINITION_FORMATION_WITH_SPECIFIED_SOURCE ( 'ANY', '', #4839, .NOT_KNOWN. ) ;
#6020 = EDGE_LOOP ( 'NONE', ( #2280, #6471, #3536 ) ) ;
#6021 = ORIENTED_EDGE ( 'NONE', *, *, #3809, .F. ) ;
#6022 = ORIENTED_EDGE ( 'NONE', *, *, #2075, .T. ) ;
#6023 = VECTOR ( 'NONE', #6353, 1000.000000000000000 ) ;
#6024 = DIRECTION ( 'NONE',  ( 0.000000000000000000, 0.4999999999999991118, -0.8660254037844391517 ) ) ;
#6025 = CARTESIAN_POINT ( 'NONE',  ( 0.4564736065166624668, -6.999999999999996447, 8.000000000000044409 ) ) ;
#6026 = DIRECTION ( 'NONE',  ( 0.000000000000000000, 0.000000000000000000, 1.000000000000000000 ) ) ;
#6027 = EDGE_LOOP ( 'NONE', ( #2745, #5468, #3260, #6440 ) ) ;
#6028 = CARTESIAN_POINT ( 'NONE',  ( -4.000000000000000000, -2.309401076758525573, -2.700000000000000178 ) ) ;
#6029 = DIRECTION ( 'NONE',  ( 1.000000000000000000, 0.000000000000000000, 0.000000000000000000 ) ) ;
#6030 = EDGE_CURVE ( 'NONE', #1769, #4218, #3392, .T. ) ;
#6031 = EDGE_CURVE ( 'NONE', #3952, #6185, #7399, .T. ) ;
#6032 = DIRECTION ( 'NONE',  ( -1.000000000000000000, 0.000000000000000000, 0.000000000000000000 ) ) ;
#6033 = SURFACE_SIDE_STYLE ('',( #7284 ) ) ;
#6034 = ADVANCED_FACE ( 'NONE', ( #2272 ), #2185, .F. ) ;
#6035 = CARTESIAN_POINT ( 'NONE',  ( -31.74999999999995737, 0.000000000000000000, 0.000000000000000000 ) ) ;
#6036 = PLANE ( 'NONE',  #5228 ) ;
#6037 = VERTEX_POINT ( 'NONE', #4221 ) ;
#6038 = ORIENTED_EDGE ( 'NONE', *, *, #1318, .F. ) ;
#6039 = AXIS2_PLACEMENT_3D ( 'NONE', #7401, #2382, #7980 ) ;
#6040 = CARTESIAN_POINT ( 'NONE',  ( -39.99999999999999289, 40.00000000000000711, 10.00000000000000000 ) ) ;
#6041 = CARTESIAN_POINT ( 'NONE',  ( 0.000000000000000000, 0.000000000000000000, -2.700000000000001066 ) ) ;
#6042 = CARTESIAN_POINT ( 'NONE',  ( 0.1999999999999987899, 0.000000000000000000, 0.000000000000000000 ) ) ;
#6043 = DIRECTION ( 'NONE',  ( -0.000000000000000000, -0.000000000000000000, 1.000000000000000000 ) ) ;
#6044 = FACE_OUTER_BOUND ( 'NONE', #5662, .T. ) ;
#6045 = CARTESIAN_POINT ( 'NONE',  ( -49.94550380033327031, 82.66312158132822674, 0.6298752594700357532 ) ) ;
#6046 = CARTESIAN_POINT ( 'NONE',  ( -54.99999999999990052, 7.999999999999996447, 13.34999999999877573 ) ) ;
#6047 = ORIENTED_EDGE ( 'NONE', *, *, #1556, .F. ) ;
#6048 = CIRCLE ( 'NONE', #3403, 1.649999999999995248 ) ;
#6049 = CARTESIAN_POINT ( 'NONE',  ( 1.300000000000000044, 1.478016689125442484, -1.626303258728256651E-15 ) ) ;
#6050 = TOROIDAL_SURFACE ( 'NONE', #4475, 2.200000000000001066, 0.2000000000000000111 ) ;
#6051 = B_SPLINE_CURVE_WITH_KNOTS ( 'NONE', 3,
 ( #2026, #19, #7115, #6334, #638, #1904, #6382, #3932, #1432, #55, #3267, #1358, #138, #1981, #5225, #2678, #4430, #3189, #5763, #685, #6419, #6449, #1268, #720 ),
 .UNSPECIFIED., .F., .F.,
 ( 4, 2, 2, 2, 2, 2, 2, 2, 2, 2, 2, 4 ),
 ( 0.006106748147956165065, 0.006869861680660866755, 0.007632975213365568445, 0.008396088746070271003, 0.009159202278774973560, 0.009540759045127317900, 0.009922315811479662240, 0.01030387257783200658, 0.01068542934418435265, 0.01106698611053669699, 0.01144854287688904307, 0.01221165640959370746 ),
 .UNSPECIFIED. ) ;
#6052 = ORIENTED_EDGE ( 'NONE', *, *, #7860, .T. ) ;
#6053 = ORIENTED_EDGE ( 'NONE', *, *, #5633, .T. ) ;
#6054 = EDGE_LOOP ( 'NONE', ( #1728, #7292, #4550, #7321, #1724 ) ) ;
#6055 = DIRECTION ( 'NONE',  ( -0.000000000000000000, 1.000000000000000000, -0.000000000000000000 ) ) ;
#6056 = CARTESIAN_POINT ( 'NONE',  ( 0.000000000000000000, 1.773042676681340968, -2.276824562219559311E-15 ) ) ;
#6057 = EDGE_CURVE ( 'NONE', #6897, #6466, #1444, .T. ) ;
#6058 = DIRECTION ( 'NONE',  ( 0.000000000000000000, 0.000000000000000000, 1.000000000000000000 ) ) ;
#6059 = CARTESIAN_POINT ( 'NONE',  ( -27.34999999999999076, 30.00000000000000711, 1.734723475976807094E-15 ) ) ;
#6060 = APPLICATION_PROTOCOL_DEFINITION ( 'draft international standard', 'automotive_design', 1998, #3646 ) ;
#6061 = EDGE_CURVE ( 'NONE', #3736, #3287, #7868, .T. ) ;
#6062 = VERTEX_POINT ( 'NONE', #4764 ) ;
#6063 = EDGE_LOOP ( 'NONE', ( #200, #7026, #2914, #5091 ) ) ;
#6064 = ORIENTED_EDGE ( 'NONE', *, *, #3219, .T. ) ;
#6065 = DIRECTION ( 'NONE',  ( -0.000000000000000000, -0.000000000000000000, 1.000000000000000000 ) ) ;
#6066 = CARTESIAN_POINT ( 'NONE',  ( 0.1999999999999987899, 0.000000000000000000, 3.500000000000000000 ) ) ;
#6067 = DIRECTION ( 'NONE',  ( -0.000000000000000000, -0.000000000000000000, 1.000000000000000000 ) ) ;
#6068 = TOROIDAL_SURFACE ( 'NONE', #8188, 1.600000000000000311, 0.1000000000000000056 ) ;
#6069 = AXIS2_PLACEMENT_3D ( 'NONE', #8080, #4522, #7085 ) ;
#6070 = ORIENTED_EDGE ( 'NONE', *, *, #4238, .T. ) ;
#6071 = CARTESIAN_POINT ( 'NONE',  ( 20.00000000000000355, 0.000000000000000000, 1.610000000000000098 ) ) ;
#6072 = EDGE_LOOP ( 'NONE', ( #4929, #1012 ) ) ;
#6073 = AXIS2_PLACEMENT_3D ( 'NONE', #3530, #6017, #2909 ) ;
#6074 = ADVANCED_FACE ( 'NONE', ( #6710 ), #345, .T. ) ;
#6075 = AXIS2_PLACEMENT_3D ( 'NONE', #1388, #2198, #3920 ) ;
#6076 = FACE_OUTER_BOUND ( 'NONE', #3929, .T. ) ;
#6077 = DIRECTION ( 'NONE',  ( -1.000000000000000000, 0.000000000000000000, 0.000000000000000000 ) ) ;
#6078 = VECTOR ( 'NONE', #5669, 1000.000000000000000 ) ;
#6079 = LINE ( 'NONE', #6163, #2922 ) ;
#6080 = AXIS2_PLACEMENT_3D ( 'NONE', #4358, #3790, #8042 ) ;
#6081 = CARTESIAN_POINT ( 'NONE',  ( 4.789799635567774772, 5.109788315999669095, 8.015886577605016328 ) ) ;
#6082 = AXIS2_PLACEMENT_3D ( 'NONE', #3939, #3022, #1150 ) ;
#6083 = AXIS2_PLACEMENT_3D ( 'NONE', #475, #3012, #2482 ) ;
#6084 = EDGE_CURVE ( 'NONE', #1617, #3952, #1708, .T. ) ;
#6085 = ORIENTED_EDGE ( 'NONE', *, *, #3329, .F. ) ;
#6086 = ORIENTED_EDGE ( 'NONE', *, *, #6204, .T. ) ;
#6087 = DIRECTION ( 'NONE',  ( 1.000000000000000000, 0.000000000000000000, 0.000000000000000000 ) ) ;
#6088 = CARTESIAN_POINT ( 'NONE',  ( 2.500000000000002220, 0.000000000000000000, 2.041999999999999815 ) ) ;
#6089 = CIRCLE ( 'NONE', #6233, 1.649999999999995248 ) ;
#6090 = CARTESIAN_POINT ( 'NONE',  ( -41.98889744358045562, 85.99540011155023933, -2.198607263777251575 ) ) ;
#6091 = CARTESIAN_POINT ( 'NONE',  ( 9.020562075079396891E-14, 10.00000000000000000, 729.2499999999977263 ) ) ;
#6092 = CARTESIAN_POINT ( 'NONE',  ( 52.00000000000000711, 8.000000000000000000, -8.000000000000000000 ) ) ;
#6093 = AXIS2_PLACEMENT_3D ( 'NONE', #1991, #2649, #6499 ) ;
#6094 = CARTESIAN_POINT ( 'NONE',  ( 1.155036213957052500E-14, 4.618802153517020059, -2.700000000000000178 ) ) ;
#6095 = ORIENTED_EDGE ( 'NONE', *, *, #4303, .T. ) ;
#6096 = LINE ( 'NONE', #1572, #473 ) ;
#6097 = ORIENTED_EDGE ( 'NONE', *, *, #3763, .T. ) ;
#6099 = EDGE_CURVE ( 'NONE', #3165, #2846, #7458, .T. ) ;
#6098 = CIRCLE ( 'NONE', #4394, 4.999999999999993783 ) ;
#6100 = ORIENTED_EDGE ( 'NONE', *, *, #4481, .T. ) ;
#6101 = CIRCLE ( 'NONE', #5958, 2.000000000000000888 ) ;
#6102 = DIRECTION ( 'NONE',  ( -0.000000000000000000, -1.000000000000000000, -0.000000000000000000 ) ) ;
#6103 = CARTESIAN_POINT ( 'NONE',  ( -52.00000000000006395, 7.999999999999996447, 11.99999999999998934 ) ) ;
#6104 = DIRECTION ( 'NONE',  ( -1.000000000000000000, -0.000000000000000000, -0.000000000000000000 ) ) ;
#6105 = CARTESIAN_POINT ( 'NONE',  ( 2.500000000000002220, -2.357898499370430834, 3.469446951953614189E-15 ) ) ;
#6106 = DIRECTION ( 'NONE',  ( 0.000000000000000000, 0.000000000000000000, 1.000000000000000000 ) ) ;
#6107 = CONICAL_SURFACE ( 'NONE', #3997, 4.000000000000000000, 1.047197551196595855 ) ;
#6108 = CONTEXT_DEPENDENT_SHAPE_REPRESENTATION ( #1188, #8012 ) ;
#6109 = ADVANCED_FACE ( 'NONE', ( #5517 ), #1742, .F. ) ;
#6110 = AXIS2_PLACEMENT_3D ( 'NONE', #5647, #6880, #3645 ) ;
#6111 = AXIS2_PLACEMENT_3D ( 'NONE', #1010, #7411, #6702 ) ;
#6112 = ORIENTED_EDGE ( 'NONE', *, *, #6126, .T. ) ;
#6113 = ORIENTED_EDGE ( 'NONE', *, *, #7764, .T. ) ;
#6114 = ORIENTED_EDGE ( 'NONE', *, *, #3897, .F. ) ;
#6115 = LINE ( 'NONE', #7487, #4517 ) ;
#6116 = DIRECTION ( 'NONE',  ( -1.000000000000000000, -0.000000000000000000, -0.000000000000000000 ) ) ;
#6117 = DIRECTION ( 'NONE',  ( -0.000000000000000000, 1.100686371591861952E-15, 1.000000000000000000 ) ) ;
#6118 = UNCERTAINTY_MEASURE_WITH_UNIT (LENGTH_MEASURE( 1.000000000000000082E-05 ), #1271, 'distance_accuracy_value', 'NONE');
#6119 = ORIENTED_EDGE ( 'NONE', *, *, #6508, .T. ) ;
#6120 = CARTESIAN_POINT ( 'NONE',  ( 3.000000000000000888, 35.09008114612887397, 4.000000000000000000 ) ) ;
#6121 = ORIENTED_EDGE ( 'NONE', *, *, #5102, .T. ) ;
#6122 = ORIENTED_EDGE ( 'NONE', *, *, #3595, .T. ) ;
#6123 = DIRECTION ( 'NONE',  ( -0.000000000000000000, -0.000000000000000000, 1.000000000000000000 ) ) ;
#6124 = DIRECTION ( 'NONE',  ( -0.000000000000000000, -0.000000000000000000, -1.000000000000000000 ) ) ;
#6125 = DIRECTION ( 'NONE',  ( 1.000000000000000000, 0.000000000000000000, 0.000000000000000000 ) ) ;
#6126 = EDGE_CURVE ( 'NONE', #4097, #1429, #5604, .T. ) ;
#6127 = DIRECTION ( 'NONE',  ( 1.000000000000000000, 0.000000000000000000, 0.000000000000000000 ) ) ;
#6128 = ADVANCED_FACE ( 'NONE', ( #4983, #1321, #1913, #2438, #2529, #7633 ), #3153, .T. ) ;
#6129 = AXIS2_PLACEMENT_3D ( 'NONE', #5616, #1248, #4449 ) ;
#6130 = ORIENTED_EDGE ( 'NONE', *, *, #572, .F. ) ;
#6131 = ORIENTED_EDGE ( 'NONE', *, *, #6504, .F. ) ;
#6132 = FACE_OUTER_BOUND ( 'NONE', #65, .T. ) ;
#6133 = CARTESIAN_POINT ( 'NONE',  ( -3.673643420401911275, -2.497823135841289677, -0.2484800633750113841 ) ) ;
#6134 = DIRECTION ( 'NONE',  ( 0.000000000000000000, 0.000000000000000000, -1.000000000000000000 ) ) ;
#6135 = DIRECTION ( 'NONE',  ( -0.000000000000000000, -0.000000000000000000, 1.000000000000000000 ) ) ;
#6136 = LINE ( 'NONE', #8036, #8174 ) ;
#6137 = ORIENTED_EDGE ( 'NONE', *, *, #5876, .T. ) ;
#6138 = ORIENTED_EDGE ( 'NONE', *, *, #6189, .T. ) ;
#6139 = CARTESIAN_POINT ( 'NONE',  ( 1.274374112546295138E-14, 85.00000000000017053, 2.000000000000043521 ) ) ;
#6140 = DIRECTION ( 'NONE',  ( 0.000000000000000000, 0.000000000000000000, 1.000000000000000000 ) ) ;
#6141 = DIRECTION ( 'NONE',  ( 0.000000000000000000, 0.000000000000000000, -1.000000000000000000 ) ) ;
#6142 = CARTESIAN_POINT ( 'NONE',  ( 0.000000000000000000, 4.163799117101000559E-16, -3.299999999999999822 ) ) ;
#6143 = ADVANCED_FACE ( 'NONE', ( #5114 ), #6261, .T. ) ;
#6144 = DIRECTION ( 'NONE',  ( -0.000000000000000000, -0.000000000000000000, -1.000000000000000000 ) ) ;
#6145 = ORIENTED_EDGE ( 'NONE', *, *, #5952, .T. ) ;
#6146 = EDGE_LOOP ( 'NONE', ( #6316, #3841, #5515, #4959 ) ) ;
#6147 = ORIENTED_EDGE ( 'NONE', *, *, #174, .T. ) ;
#6148 = PLANE ( 'NONE',  #7940 ) ;
#6149 = DIRECTION ( 'NONE',  ( -0.7071067811865310304, 0.000000000000000000, 0.7071067811865641151 ) ) ;
#6150 = CARTESIAN_POINT ( 'NONE',  ( -52.00000000000006395, 7.999999999999996447, 11.99999999999998934 ) ) ;
#6151 = ADVANCED_BREP_SHAPE_REPRESENTATION ( '', ( #6901, #1587 ), #6006 ) ;
#6152 = MECHANICAL_DESIGN_GEOMETRIC_PRESENTATION_REPRESENTATION (  '', ( #7745 ), #2053 ) ;
#6153 = EDGE_CURVE ( 'NONE', #7658, #2258, #5020, .T. ) ;
#6154 =( LENGTH_UNIT ( ) NAMED_UNIT ( * ) SI_UNIT ( .MILLI., .METRE. ) );
#6155 = ORIENTED_EDGE ( 'NONE', *, *, #7948, .F. ) ;
#6156 = CARTESIAN_POINT ( 'NONE',  ( 39.83716857408421674, 108.0000000000001990, -4.999999999999976907 ) ) ;
#6157 = ORIENTED_EDGE ( 'NONE', *, *, #1350, .T. ) ;
#6158 = AXIS2_PLACEMENT_3D ( 'NONE', #1408, #731, #5739 ) ;
#6159 = ORIENTED_EDGE ( 'NONE', *, *, #6362, .F. ) ;
#6160 = CARTESIAN_POINT ( 'NONE',  ( -2.999999999999998668, 35.09008114612887397, 4.000000000000000000 ) ) ;
#6161 = CARTESIAN_POINT ( 'NONE',  ( -41.93505285506407887, 82.66506966722154459, 0.5694876689910105538 ) ) ;
#6162 = EDGE_CURVE ( 'NONE', #2562, #6538, #3682, .T. ) ;
#6163 = CARTESIAN_POINT ( 'NONE',  ( 25.00000000000001421, -29.99999999999997868, 10.00000000000000000 ) ) ;
#6164 = LINE ( 'NONE', #8073, #2425 ) ;
#6165 = ORIENTED_EDGE ( 'NONE', *, *, #4520, .F. ) ;
#6166 = ORIENTED_EDGE ( 'NONE', *, *, #7455, .F. ) ;
#6167 = SURFACE_STYLE_USAGE ( .BOTH. , #7503 ) ;
#6168 = EDGE_CURVE ( 'NONE', #4218, #166, #2102, .T. ) ;
#6169 = CARTESIAN_POINT ( 'NONE',  ( 3.999999999999997335, 0.000000000000000000, -2.200000000000001066 ) ) ;
#6170 = DIRECTION ( 'NONE',  ( 0.000000000000000000, -1.000000000000000000, 9.783878858594330870E-16 ) ) ;
#6171 = CARTESIAN_POINT ( 'NONE',  ( 0.000000000000000000, 0.000000000000000000, -2.394516984716111185 ) ) ;
#6172 = CARTESIAN_POINT ( 'NONE',  ( 42.00000000000003553, 85.00000000000012790, -5.000000000000003553 ) ) ;
#6173 = CARTESIAN_POINT ( 'NONE',  ( 0.000000000000000000, 0.000000000000000000, 3.851859888774471706E-31 ) ) ;
#6174 = ORIENTED_EDGE ( 'NONE', *, *, #7782, .T. ) ;
#6175 = VERTEX_POINT ( 'NONE', #6879 ) ;
#6176 = CARTESIAN_POINT ( 'NONE',  ( 1.300000000000000044, 0.7390083445627193548, -1.280000000000000693 ) ) ;
#6177 = DIRECTION ( 'NONE',  ( 0.000000000000000000, 0.000000000000000000, 1.000000000000000000 ) ) ;
#6178 = DIRECTION ( 'NONE',  ( -1.000000000000000000, 0.000000000000000000, -0.000000000000000000 ) ) ;
#6179 = CARTESIAN_POINT ( 'NONE',  ( 2.500000000000002220, 0.000000000000000000, 0.000000000000000000 ) ) ;
#6180 = LINE ( 'NONE', #7435, #4506 ) ;
#6181 = DIRECTION ( 'NONE',  ( 0.000000000000000000, 0.000000000000000000, 1.000000000000000000 ) ) ;
#6182 = AXIS2_PLACEMENT_3D ( 'NONE', #7997, #2856, #6583 ) ;
#6183 = ITEM_DEFINED_TRANSFORMATION ( 'NONE', 'NONE', #1111,  #1587 ) ;
#6184 = ORIENTED_EDGE ( 'NONE', *, *, #4415, .F. ) ;
#6185 = VERTEX_POINT ( 'NONE', #6169 ) ;
#6186 = PRODUCT_DEFINITION ( 'UNKNOWN', '', #4686, #4417 ) ;
#6187 = ORIENTED_EDGE ( 'NONE', *, *, #2430, .F. ) ;
#6188 = VERTEX_POINT ( 'NONE', #6212 ) ;
#6189 = EDGE_CURVE ( 'NONE', #741, #3745, #4478, .T. ) ;
#6190 = EDGE_CURVE ( 'NONE', #2318, #5123, #6595, .T. ) ;
#6191 = DIRECTION ( 'NONE',  ( -1.000000000000000000, 0.000000000000000000, 2.224004456380520794E-17 ) ) ;
#6192 = CARTESIAN_POINT ( 'NONE',  ( 57.99999999999999289, 7.999999999999996447, 19.99999999999998934 ) ) ;
#6193 = CARTESIAN_POINT ( 'NONE',  ( 0.000000000000000000, 0.000000000000000000, -2.700000000000000178 ) ) ;
#6194 = EDGE_LOOP ( 'NONE', ( #3768, #3689, #1698, #1819 ) ) ;
#6195 = CARTESIAN_POINT ( 'NONE',  ( 2.500000000000002220, -2.357898499370430834, 3.469446951953614189E-15 ) ) ;
#6196 = EDGE_LOOP ( 'NONE', ( #3484, #6811, #7331 ) ) ;
#6197 = EDGE_LOOP ( 'NONE', ( #2941, #2746, #2920, #518, #4001, #1048 ) ) ;
#6198 = AXIS2_PLACEMENT_3D ( 'NONE', #5797, #4431, #5764 ) ;
#6199 = DIRECTION ( 'NONE',  ( -0.000000000000000000, -0.000000000000000000, 1.000000000000000000 ) ) ;
#6200 = LINE ( 'NONE', #4298, #7423 ) ;
#6201 = PRESENTATION_LAYER_ASSIGNMENT (  '', '', ( #1557 ) ) ;
#6202 = CARTESIAN_POINT ( 'NONE',  ( -39.83716857408418122, 108.0000000000001990, -4.999999999999976907 ) ) ;
#6203 = VECTOR ( 'NONE', #8137, 1000.000000000000114 ) ;
#6204 = EDGE_CURVE ( 'NONE', #6473, #6416, #6356, .T. ) ;
#6205 = DIRECTION ( 'NONE',  ( 0.000000000000000000, 0.5000000000000011102, 0.8660254037844380415 ) ) ;
#6206 = AXIS2_PLACEMENT_3D ( 'NONE', #3362, #4568, #7754 ) ;
#6207 = AXIS2_PLACEMENT_3D ( 'NONE', #2555, #676, #6322 ) ;
#6208 = EDGE_CURVE ( 'NONE', #5767, #4563, #3180, .T. ) ;
#6209 = ORIENTED_EDGE ( 'NONE', *, *, #5481, .F. ) ;
#6210 = EDGE_LOOP ( 'NONE', ( #3020, #2527, #2670 ) ) ;
#6211 = CARTESIAN_POINT ( 'NONE',  ( 0.1999999999999987899, 0.000000000000000000, 0.000000000000000000 ) ) ;
#6212 = CARTESIAN_POINT ( 'NONE',  ( 0.000000000000000000, 0.7390083445627224634, 1.279999999999999138 ) ) ;
#6213 = DIRECTION ( 'NONE',  ( 0.000000000000000000, 0.4999999999999992784, -0.8660254037844390407 ) ) ;
#6214 = VECTOR ( 'NONE', #2836, 1000.000000000000000 ) ;
#6215 = LINE ( 'NONE', #5561, #2659 ) ;
#6216 = AXIS2_PLACEMENT_3D ( 'NONE', #5694, #6354, #6891 ) ;
#6217 = CIRCLE ( 'NONE', #7147, 2.700000000000000622 ) ;
#6218 = CARTESIAN_POINT ( 'NONE',  ( 41.08716857408421674, 108.0000000000001990, -4.999999999999976907 ) ) ;
#6219 = AXIS2_PLACEMENT_3D ( 'NONE', #1204, #3746, #2322 ) ;
#6220 = DIRECTION ( 'NONE',  ( 0.000000000000000000, -0.4999999999999992228, 0.8660254037844390407 ) ) ;
#6221 = ORIENTED_EDGE ( 'NONE', *, *, #4261, .F. ) ;
#6222 = ORIENTED_EDGE ( 'NONE', *, *, #3316, .T. ) ;
#6223 = AXIS2_PLACEMENT_3D ( 'NONE', #5497, #6777, #995 ) ;
#6224 = DIRECTION ( 'NONE',  ( 0.000000000000000000, 0.000000000000000000, -1.000000000000000000 ) ) ;
#6225 = COLOUR_RGB ( '', 0.09019608, 0.27058824, 0.51372549) ;
#6226 = CARTESIAN_POINT ( 'NONE',  ( 3.345653888883671545, -2.687187980154741140, -2.560849780464844905 ) ) ;
#6227 = CARTESIAN_POINT ( 'NONE',  ( -2.500000000000002220, 0.000000000000000000, -2.674599999999998978 ) ) ;
#6228 = DIRECTION ( 'NONE',  ( -1.412205397084881070E-17, 2.775557561562891967E-17, 1.000000000000000000 ) ) ;
#6229 = CARTESIAN_POINT ( 'NONE',  ( 1.284259550325887758E-14, 85.00000000000005684, -5.000000000000004441 ) ) ;
#6230 = CARTESIAN_POINT ( 'NONE',  ( -31.74999999999995737, 0.000000000000000000, 0.000000000000000000 ) ) ;
#6231 = VECTOR ( 'NONE', #6317, 1000.000000000000000 ) ;
#6232 = ORIENTED_EDGE ( 'NONE', *, *, #1274, .F. ) ;
#6233 = AXIS2_PLACEMENT_3D ( 'NONE', #54, #684, #1903 ) ;
#6234 = EDGE_CURVE ( 'NONE', #4539, #6012, #4400, .T. ) ;
#6235 = AXIS2_PLACEMENT_3D ( 'NONE', #7193, #5413, #4738 ) ;
#6236 = ORIENTED_EDGE ( 'NONE', *, *, #7470, .T. ) ;
#6237 = ADVANCED_FACE ( 'NONE', ( #605 ), #6304, .T. ) ;
#6238 = ORIENTED_EDGE ( 'NONE', *, *, #3860, .T. ) ;
#6239 = EDGE_LOOP ( 'NONE', ( #993, #2267, #7267 ) ) ;
#6240 = PRODUCT_DEFINITION_SHAPE ( 'NONE', 'NONE',  #8217 ) ;
#6241 = CIRCLE ( 'NONE', #5847, 4.000000000000000888 ) ;
#6242 = CARTESIAN_POINT ( 'NONE',  ( 60.00000000000000711, 10.00000000000000000, 0.000000000000000000 ) ) ;
#6243 = AXIS2_PLACEMENT_3D ( 'NONE', #4250, #414, #3712 ) ;
#6244 = DIRECTION ( 'NONE',  ( -0.000000000000000000, -0.000000000000000000, 1.000000000000000000 ) ) ;
#6245 = SURFACE_STYLE_FILL_AREA ( #1168 ) ;
#6246 = VERTEX_POINT ( 'NONE', #649 ) ;
#6247 = DIRECTION ( 'NONE',  ( 0.000000000000000000, -1.000000000000000000, 0.000000000000000000 ) ) ;
#6248 = ORIENTED_EDGE ( 'NONE', *, *, #220, .F. ) ;
#6249 = ORIENTED_EDGE ( 'NONE', *, *, #6966, .F. ) ;
#6250 = CARTESIAN_POINT ( 'NONE',  ( 2.000000000000000000, 0.000000000000000000, 0.000000000000000000 ) ) ;
#6251 = CARTESIAN_POINT ( 'NONE',  ( -42.00000000000000711, 85.00000000000011369, -2.399999999999999911 ) ) ;
#6252 = CARTESIAN_POINT ( 'NONE',  ( 10.00000000000000000, 1.224646799147353256E-15, 18.00000000000000355 ) ) ;
#6253 = EDGE_CURVE ( 'NONE', #1485, #3745, #3198, .T. ) ;
#6254 = LINE ( 'NONE', #4840, #3466 ) ;
#6255 = EDGE_CURVE ( 'NONE', #4814, #2960, #2399, .T. ) ;
#6256 = FACE_OUTER_BOUND ( 'NONE', #5674, .T. ) ;
#6257 = EDGE_LOOP ( 'NONE', ( #7442, #1087, #3765, #7596, #86, #1977 ) ) ;
#6258 = ORIENTED_EDGE ( 'NONE', *, *, #2561, .T. ) ;
#6259 = EDGE_CURVE ( 'NONE', #792, #5998, #6834, .T. ) ;
#6260 = LINE ( 'NONE', #3107, #5549 ) ;
#6261 = CYLINDRICAL_SURFACE ( 'NONE', #4886, 2.000000000000000888 ) ;
#6262 = LINE ( 'NONE', #606, #1045 ) ;
#6263 = CARTESIAN_POINT ( 'NONE',  ( 4.000000000000000000, 3.500000000000000000, 0.000000000000000000 ) ) ;
#6264 = EDGE_CURVE ( 'NONE', #2250, #7927, #2238, .T. ) ;
#6265 = DIRECTION ( 'NONE',  ( -1.000000000000000000, 0.000000000000000000, 0.000000000000000000 ) ) ;
#6266 = DIRECTION ( 'NONE',  ( -0.000000000000000000, 0.000000000000000000, 1.000000000000000000 ) ) ;
#6267 = AXIS2_PLACEMENT_3D ( 'NONE', #2544, #5087, #6141 ) ;
#6268 = ORIENTED_EDGE ( 'NONE', *, *, #2740, .F. ) ;
#6269 = PLANE ( 'NONE',  #5373 ) ;
#6270 = PLANE ( 'NONE',  #1994 ) ;
#6271 = LINE ( 'NONE', #1921, #1857 ) ;
#6272 = CARTESIAN_POINT ( 'NONE',  ( 57.99999999999999289, -8.000000000000001776, 19.99999999999998224 ) ) ;
#6273 = AXIS2_PLACEMENT_3D ( 'NONE', #1139, #6748, #6205 ) ;
#6274 = DIRECTION ( 'NONE',  ( 1.000000000000000000, 0.000000000000000000, 0.000000000000000000 ) ) ;
#6275 = CARTESIAN_POINT ( 'NONE',  ( 49.96747517473578881, 86.80656978053562511, 1.587697219280558958 ) ) ;
#6276 = EDGE_LOOP ( 'NONE', ( #5047, #5665, #6923, #3594, #6145 ) ) ;
#6277 = ORIENTED_EDGE ( 'NONE', *, *, #3146, .T. ) ;
#6278 = DIRECTION ( 'NONE',  ( 0.000000000000000000, 0.000000000000000000, 1.000000000000000000 ) ) ;
#6279 = EDGE_LOOP ( 'NONE', ( #5446, #6064, #1254, #1851 ) ) ;
#6280 = ORIENTED_EDGE ( 'NONE', *, *, #2587, .F. ) ;
#6281 = CARTESIAN_POINT ( 'NONE',  ( 30.00000000000000000, 0.000000000000000000, -6.938893903907228378E-15 ) ) ;
#6282 = CARTESIAN_POINT ( 'NONE',  ( 40.00000000000000711, -39.99999999999999289, 10.00000000000000000 ) ) ;
#6283 = DIRECTION ( 'NONE',  ( -1.000000000000000000, -0.000000000000000000, -0.000000000000000000 ) ) ;
#6284 =( GEOMETRIC_REPRESENTATION_CONTEXT ( 3 ) GLOBAL_UNCERTAINTY_ASSIGNED_CONTEXT ( ( #6779 ) ) GLOBAL_UNIT_ASSIGNED_CONTEXT ( ( #599, #4974, #1136 ) ) REPRESENTATION_CONTEXT ( 'NONE', 'WORKASPACE' ) );
#6285 = ORIENTED_EDGE ( 'NONE', *, *, #6030, .T. ) ;
#6286 = CARTESIAN_POINT ( 'NONE',  ( 49.98887975752123936, 83.93556181870177113, -2.156785159512917716 ) ) ;
#6287 =( REPRESENTATION_RELATIONSHIP ('NONE','NONE', #3916, #1314 ) REPRESENTATION_RELATIONSHIP_WITH_TRANSFORMATION ( #6809 )SHAPE_REPRESENTATION_RELATIONSHIP( ) );
#6288 = EDGE_LOOP ( 'NONE', ( #2416, #4230 ) ) ;
#6289 = ORIENTED_EDGE ( 'NONE', *, *, #5004, .T. ) ;
#6290 = PRESENTATION_LAYER_ASSIGNMENT (  '', '', ( #7490 ) ) ;
#6291 = LINE ( 'NONE', #5144, #5434 ) ;
#6292 = LINE ( 'NONE', #5678, #5715 ) ;
#6293 = LINE ( 'NONE', #3190, #7913 ) ;
#6294 = ADVANCED_FACE ( 'NONE', ( #5151 ), #6390, .F. ) ;
#6295 = SURFACE_STYLE_USAGE ( .BOTH. , #425 ) ;
#6296 = DIRECTION ( 'NONE',  ( 0.000000000000000000, 0.000000000000000000, -1.000000000000000000 ) ) ;
#6297 = FACE_BOUND ( 'NONE', #7452, .T. ) ;
#6298 = EDGE_CURVE ( 'NONE', #7616, #3227, #3864, .T. ) ;
#6299 = EDGE_LOOP ( 'NONE', ( #1927, #2998 ) ) ;
#6300 = EDGE_LOOP ( 'NONE', ( #1059, #2153, #7462, #1748 ) ) ;
#6301 = EDGE_CURVE ( 'NONE', #5320, #7674, #1576, .T. ) ;
#6302 = EDGE_CURVE ( 'NONE', #5106, #4097, #231, .T. ) ;
#6303 = CARTESIAN_POINT ( 'NONE',  ( -1.249999999999992895, 38.99999999999999289, -4.999999999999990230 ) ) ;
#6304 = CYLINDRICAL_SURFACE ( 'NONE', #5168, 10.00000000000000000 ) ;
#6305 = LINE ( 'NONE', #1280, #6366 ) ;
#6306 = CARTESIAN_POINT ( 'NONE',  ( 4.999999999999993783, 6.123233995736758394E-16, 0.000000000000000000 ) ) ;
#6307 = DIRECTION ( 'NONE',  ( 0.000000000000000000, -1.000000000000000000, 0.000000000000000000 ) ) ;
#6308 = FACE_OUTER_BOUND ( 'NONE', #4758, .T. ) ;
#6309 = ORIENTED_EDGE ( 'NONE', *, *, #6084, .F. ) ;
#6310 = DIRECTION ( 'NONE',  ( -1.000000000000000000, 0.000000000000000000, -0.000000000000000000 ) ) ;
#6311 = FACE_OUTER_BOUND ( 'NONE', #2501, .T. ) ;
#6312 = FACE_BOUND ( 'NONE', #4652, .T. ) ;
#6313 = FACE_OUTER_BOUND ( 'NONE', #2898, .T. ) ;
#6314 = CARTESIAN_POINT ( 'NONE',  ( 49.95669389512431025, 87.08239168930832363, 1.203442334140423231 ) ) ;
#6315 = ORIENTED_EDGE ( 'NONE', *, *, #5105, .F. ) ;
#6316 = ORIENTED_EDGE ( 'NONE', *, *, #7776, .F. ) ;
#6317 = DIRECTION ( 'NONE',  ( -0.000000000000000000, -1.000000000000000000, -0.000000000000000000 ) ) ;
#6318 = EDGE_LOOP ( 'NONE', ( #794, #4484 ) ) ;
#6319 = ADVANCED_FACE ( 'NONE', ( #2906 ), #8065, .F. ) ;
#6320 = ORIENTED_EDGE ( 'NONE', *, *, #398, .T. ) ;
#6321 = CONICAL_SURFACE ( 'NONE', #8030, 2.500000000000002220, 0.9599310885968777018 ) ;
#6322 = DIRECTION ( 'NONE',  ( 0.000000000000000000, 0.000000000000000000, -1.000000000000000000 ) ) ;
#6323 = CARTESIAN_POINT ( 'NONE',  ( 1.300000000000000044, 1.567547902908612085E-16, -1.280000000000000027 ) ) ;
#6324 = CARTESIAN_POINT ( 'NONE',  ( 38.58716857408421674, 108.0000000000001990, -4.999999999999976907 ) ) ;
#6325 = CARTESIAN_POINT ( 'NONE',  ( 6.424279303448175372E-15, 46.01196202519845002, -3.375579649125778804E-15 ) ) ;
#6326 = EDGE_CURVE ( 'NONE', #580, #8077, #7384, .T. ) ;
#6327 = ORIENTED_EDGE ( 'NONE', *, *, #4578, .T. ) ;
#6328 = DIRECTION ( 'NONE',  ( -1.000000000000000000, 0.000000000000000000, 1.412205397084726379E-17 ) ) ;
#6329 = AXIS2_PLACEMENT_3D ( 'NONE', #5126, #2660, #4533 ) ;
#6330 = CIRCLE ( 'NONE', #2084, 3.999999999999999112 ) ;
#6331 = EDGE_LOOP ( 'NONE', ( #6404, #4334 ) ) ;
#6332 = ORIENTED_EDGE ( 'NONE', *, *, #5485, .F. ) ;
#6333 = CARTESIAN_POINT ( 'NONE',  ( 10.71950000000001424, 0.000000000000000000, 0.000000000000000000 ) ) ;
#6334 = CARTESIAN_POINT ( 'NONE',  ( 41.98889744358049114, 84.00459988845015857, -2.198607263777018872 ) ) ;
#6335 = CYLINDRICAL_SURFACE ( 'NONE', #3961, 2.649999999999999467 ) ;
#6336 = DIRECTION ( 'NONE',  ( -0.000000000000000000, -0.000000000000000000, 1.000000000000000000 ) ) ;
#6337 = EDGE_CURVE ( 'NONE', #8104, #189, #5977, .T. ) ;
#6338 = VECTOR ( 'NONE', #6450, 1000.000000000000000 ) ;
#6339 = ADVANCED_FACE ( 'NONE', ( #6721, #1662 ), #3490, .T. ) ;
#6340 = VERTEX_POINT ( 'NONE', #2242 ) ;
#6341 = CIRCLE ( 'NONE', #1306, 2.500000000000002220 ) ;
#6342 = DIRECTION ( 'NONE',  ( -0.000000000000000000, 0.000000000000000000, -1.000000000000000000 ) ) ;
#6343 = DIRECTION ( 'NONE',  ( 1.000000000000000000, -0.000000000000000000, -0.000000000000000000 ) ) ;
#6344 = CARTESIAN_POINT ( 'NONE',  ( 2.000000000000000000, 0.8865213383406685965, -1.535500000000000753 ) ) ;
#6345 = CARTESIAN_POINT ( 'NONE',  ( 0.000000000000000000, 0.000000000000000000, 5.400000000000002132 ) ) ;
#6346 = VECTOR ( 'NONE', #7296, 1000.000000000000114 ) ;
#6347 = CARTESIAN_POINT ( 'NONE',  ( 2.500000000000002220, 2.357898499370434386, -3.469446951953614189E-15 ) ) ;
#6348 = PRODUCT_RELATED_PRODUCT_CATEGORY ( 'part', '', ( #5512 ) ) ;
#6349 = AXIS2_PLACEMENT_3D ( 'NONE', #6229, #1793, #4955 ) ;
#6350 = CARTESIAN_POINT ( 'NONE',  ( -49.96738998307156265, 86.80892218194620114, 1.585032901986263454 ) ) ;
#6351 = VECTOR ( 'NONE', #4582, 1000.000000000000000 ) ;
#6352 = EDGE_LOOP ( 'NONE', ( #7738, #3581, #1147, #5960 ) ) ;
#6353 = DIRECTION ( 'NONE',  ( -0.000000000000000000, -0.000000000000000000, 1.000000000000000000 ) ) ;
#6354 = DIRECTION ( 'NONE',  ( -0.000000000000000000, -0.000000000000000000, 1.000000000000000000 ) ) ;
#6355 = PLANE ( 'NONE',  #334 ) ;
#6356 = CIRCLE ( 'NONE', #6741, 4.999999999999993783 ) ;
#6357 = AXIS2_PLACEMENT_3D ( 'NONE', #1348, #3882, #6984 ) ;
#6358 = CARTESIAN_POINT ( 'NONE',  ( 23.61000000000001364, 2.449293598294707400E-16, -2.000000000000000444 ) ) ;
#6359 = CARTESIAN_POINT ( 'NONE',  ( 49.95346081399738125, 87.15763333356291298, -1.062739361927934612 ) ) ;
#6360 = EDGE_CURVE ( 'NONE', #6761, #7783, #3224, .T. ) ;
#6361 = ORIENTED_EDGE ( 'NONE', *, *, #2989, .F. ) ;
#6362 = EDGE_CURVE ( 'NONE', #1575, #2820, #4729, .T. ) ;
#6363 = AXIS2_PLACEMENT_3D ( 'NONE', #3908, #5125, #2723 ) ;
#6364 = CIRCLE ( 'NONE', #5183, 2.041999999999999815 ) ;
#6365 = ORIENTED_EDGE ( 'NONE', *, *, #797, .F. ) ;
#6366 = VECTOR ( 'NONE', #1743, 1000.000000000000000 ) ;
#6367 = CARTESIAN_POINT ( 'NONE',  ( 42.00000000000003553, 84.88315974372717676, 2.399999999999971489 ) ) ;
#6368 = ORIENTED_EDGE ( 'NONE', *, *, #5553, .F. ) ;
#6369 = ORIENTED_EDGE ( 'NONE', *, *, #5860, .F. ) ;
#6370 = VECTOR ( 'NONE', #2, 1000.000000000000000 ) ;
#6371 = LINE ( 'NONE', #2628, #7681 ) ;
#6373 = EDGE_CURVE ( 'NONE', #2810, #3673, #317, .T. ) ;
#6372 = PLANE ( 'NONE',  #4643 ) ;
#6374 = DIRECTION ( 'NONE',  ( 0.000000000000000000, -1.000000000000000000, 9.783878858594330870E-16 ) ) ;
#6375 = CIRCLE ( 'NONE', #2778, 1.535500000000000087 ) ;
#6376 = CARTESIAN_POINT ( 'NONE',  ( 4.511103391248660453E-14, 16.01196202519795619, -6.505213034913026604E-15 ) ) ;
#6377 = ORIENTED_EDGE ( 'NONE', *, *, #2706, .F. ) ;
#6378 = VERTEX_POINT ( 'NONE', #5491 ) ;
#6379 = ORIENTED_EDGE ( 'NONE', *, *, #5759, .T. ) ;
#6380 = CIRCLE ( 'NONE', #2666, 1.599999999999986766 ) ;
#6381 = FACE_OUTER_BOUND ( 'NONE', #4354, .T. ) ;
#6382 = CARTESIAN_POINT ( 'NONE',  ( 41.96090147793651681, 83.18226251854572695, -1.587618400553736597 ) ) ;
#6383 = CARTESIAN_POINT ( 'NONE',  ( 0.1999999999999987899, 0.000000000000000000, 0.000000000000000000 ) ) ;
#6384 = SHAPE_REPRESENTATION_RELATIONSHIP ( 'NONE' , 'NONE' ,  #499, #6151 ) ;
#6385 = PRODUCT_DEFINITION_SHAPE ( 'NONE', 'NONE',  #1427 ) ;
#6386 = CARTESIAN_POINT ( 'NONE',  ( 1.284259550325887758E-14, 85.00000000000005684, -5.000000000000004441 ) ) ;
#6387 = CIRCLE ( 'NONE', #7582, 2.650000000000010125 ) ;
#6388 = ORIENTED_EDGE ( 'NONE', *, *, #4751, .F. ) ;
#6389 = DIRECTION ( 'NONE',  ( -0.000000000000000000, -0.000000000000000000, -1.000000000000000000 ) ) ;
#6390 = PLANE ( 'NONE',  #6883 ) ;
#6391 = CARTESIAN_POINT ( 'NONE',  ( 55.00000000000000000, 8.000000000000000000, -6.149999999999981704 ) ) ;
#6392 = DIRECTION ( 'NONE',  ( 0.000000000000000000, 0.000000000000000000, 1.000000000000000000 ) ) ;
#6393 = EDGE_CURVE ( 'NONE', #4453, #5852, #770, .T. ) ;
#6394 = EDGE_CURVE ( 'NONE', #5083, #4177, #3527, .T. ) ;
#6395 = CARTESIAN_POINT ( 'NONE',  ( -49.98627395458710510, 86.20659363562862154, -2.098057260256866119 ) ) ;
#6396 = ORIENTED_EDGE ( 'NONE', *, *, #5227, .F. ) ;
#6397 = DIRECTION ( 'NONE',  ( -1.000000000000000000, -0.000000000000000000, -0.000000000000000000 ) ) ;
#6398 = CARTESIAN_POINT ( 'NONE',  ( 2.000000000000000000, 0.8865213383406687075, -1.535500000000000975 ) ) ;
#6399 = CARTESIAN_POINT ( 'NONE',  ( -49.99637462046958092, 84.37866470723815837, 2.323446361670006954 ) ) ;
#6400 = AXIS2_PLACEMENT_3D ( 'NONE', #5695, #2434, #2983 ) ;
#6401 = ORIENTED_EDGE ( 'NONE', *, *, #4862, .F. ) ;
#6402 = ORIENTED_EDGE ( 'NONE', *, *, #1630, .F. ) ;
#6403 = CARTESIAN_POINT ( 'NONE',  ( -4.000000000000000000, -2.309401076758531346, -2.342734410091827701 ) ) ;
#6404 = ORIENTED_EDGE ( 'NONE', *, *, #2234, .F. ) ;
#6405 = AXIS2_PLACEMENT_3D ( 'NONE', #892, #5968, #3363 ) ;
#6406 = ORIENTED_EDGE ( 'NONE', *, *, #1230, .F. ) ;
#6407 = EDGE_CURVE ( 'NONE', #3462, #531, #4367, .T. ) ;
#6408 = EDGE_CURVE ( 'NONE', #4177, #5731, #1176, .T. ) ;
#6409 = CARTESIAN_POINT ( 'NONE',  ( -41.99055603561590289, 84.08175327132279619, 2.229652810622042125 ) ) ;
#6410 = DIRECTION ( 'NONE',  ( -1.000000000000000000, 0.000000000000000000, 0.000000000000000000 ) ) ;
#6411 = CARTESIAN_POINT ( 'NONE',  ( 2.000000000000000000, 1.773042676681340968, -2.276824562219559311E-15 ) ) ;
#6412 = DIRECTION ( 'NONE',  ( -1.000000000000000000, -5.692221470121481927E-17, 0.000000000000000000 ) ) ;
#6413 = SHAPE_REPRESENTATION ( 'mirror holder', ( #1587 ), #1249 ) ;
#6414 = ORIENTED_EDGE ( 'NONE', *, *, #5876, .F. ) ;
#6415 = EDGE_CURVE ( 'NONE', #1461, #6062, #4560, .T. ) ;
#6416 = VERTEX_POINT ( 'NONE', #2324 ) ;
#6417 = ORIENTED_EDGE ( 'NONE', *, *, #5235, .F. ) ;
#6418 = CARTESIAN_POINT ( 'NONE',  ( 2.000000000000000000, -0.8865213383406690406, 1.535500000000000975 ) ) ;
#6419 = CARTESIAN_POINT ( 'NONE',  ( 41.95400501379508285, 83.03335366937368178, 1.381527937806807271 ) ) ;
#6420 = CARTESIAN_POINT ( 'NONE',  ( 4.000000000000003553, 0.000000000000000000, 0.000000000000000000 ) ) ;
#6421 = DIRECTION ( 'NONE',  ( 0.000000000000000000, 0.000000000000000000, -1.000000000000000000 ) ) ;
#6422 = EDGE_CURVE ( 'NONE', #3881, #4768, #4630, .T. ) ;
#6423 = DIRECTION ( 'NONE',  ( 0.000000000000000000, -0.5000000000000013323, -0.8660254037844378194 ) ) ;
#6424 = LINE ( 'NONE', #2610, #4244 ) ;
#6425 = DIRECTION ( 'NONE',  ( -0.000000000000000000, -0.000000000000000000, -1.000000000000000000 ) ) ;
#6426 = MECHANICAL_DESIGN_GEOMETRIC_PRESENTATION_REPRESENTATION (  '', ( #8000 ), #5501 ) ;
#6427 = DIRECTION ( 'NONE',  ( 0.000000000000000000, 0.000000000000000000, 1.000000000000000000 ) ) ;
#6428 = CARTESIAN_POINT ( 'NONE',  ( -49.96366046868872246, 86.90794461356699685, -1.464368789226978329 ) ) ;
#6429 = AXIS2_PLACEMENT_3D ( 'NONE', #3871, #6397, #3243 ) ;
#6430 = EDGE_LOOP ( 'NONE', ( #4207, #7996, #3880, #5476 ) ) ;
#6431 = PLANE ( 'NONE',  #5506 ) ;
#6432 = LINE ( 'NONE', #4604, #3569 ) ;
#6433 = DIRECTION ( 'NONE',  ( -0.8571673007021125557, -1.430919794933845163E-16, -0.5150380749100536004 ) ) ;
#6434 = DIRECTION ( 'NONE',  ( 1.000000000000000000, 0.000000000000000000, 0.000000000000000000 ) ) ;
#6435 = CARTESIAN_POINT ( 'NONE',  ( 29.99999999999997868, 30.00000000000001421, 10.00000000000000000 ) ) ;
#6436 = ORIENTED_EDGE ( 'NONE', *, *, #1722, .F. ) ;
#6437 = ORIENTED_EDGE ( 'NONE', *, *, #752, .T. ) ;
#6438 = DIRECTION ( 'NONE',  ( -1.000000000000000000, 0.000000000000000000, 2.224004456380520794E-17 ) ) ;
#6439 = ORIENTED_EDGE ( 'NONE', *, *, #6648, .F. ) ;
#6440 = ORIENTED_EDGE ( 'NONE', *, *, #3127, .F. ) ;
#6441 = PLANE ( 'NONE',  #7015 ) ;
#6442 = DIRECTION ( 'NONE',  ( 1.000000000000000000, 0.000000000000000000, 0.000000000000000000 ) ) ;
#6443 = DIRECTION ( 'NONE',  ( -0.000000000000000000, -0.000000000000000000, 1.000000000000000000 ) ) ;
#6444 = EDGE_CURVE ( 'NONE', #3060, #7290, #4777, .T. ) ;
#6445 = ORIENTED_EDGE ( 'NONE', *, *, #6949, .F. ) ;
#6446 = ORIENTED_EDGE ( 'NONE', *, *, #4785, .T. ) ;
#6447 = ORIENTED_EDGE ( 'NONE', *, *, #6362, .T. ) ;
#6448 = DIRECTION ( 'NONE',  ( -1.000000000000000000, -0.000000000000000000, -0.000000000000000000 ) ) ;
#6449 = CARTESIAN_POINT ( 'NONE',  ( 41.96465185579614143, 83.26999058642596196, 1.682954651729509754 ) ) ;
#6450 = DIRECTION ( 'NONE',  ( 0.000000000000000000, 1.000000000000000000, -1.467581828789149532E-15 ) ) ;
#6451 = VECTOR ( 'NONE', #8147, 1000.000000000000000 ) ;
#6452 = SURFACE_STYLE_FILL_AREA ( #3936 ) ;
#6453 = CARTESIAN_POINT ( 'NONE',  ( 30.00000000000001066, -29.99999999999997868, 10.00000000000000000 ) ) ;
#6454 = DIRECTION ( 'NONE',  ( 1.000000000000000000, 0.000000000000000000, 0.000000000000000000 ) ) ;
#6455 = ADVANCED_FACE ( 'NONE', ( #6680 ), #4857, .F. ) ;
#6456 = DIRECTION ( 'NONE',  ( 1.000000000000000000, 0.000000000000000000, 0.000000000000000000 ) ) ;
#6457 = DIRECTION ( 'NONE',  ( -1.000000000000000000, -0.000000000000000000, -0.000000000000000000 ) ) ;
#6458 = ORIENTED_EDGE ( 'NONE', *, *, #1998, .T. ) ;
#6459 = FACE_OUTER_BOUND ( 'NONE', #895, .T. ) ;
#6460 = SURFACE_STYLE_USAGE ( .BOTH. , #5271 ) ;
#6461 = CARTESIAN_POINT ( 'NONE',  ( 5.200000000000020606, 0.000000000000000000, 2.499999999999993339 ) ) ;
#6462 = CIRCLE ( 'NONE', #3685, 3.500000000000000000 ) ;
#6463 = CARTESIAN_POINT ( 'NONE',  ( 24.99999999999998224, 30.00000000000001421, 10.00000000000000000 ) ) ;
#6464 = DIRECTION ( 'NONE',  ( 0.000000000000000000, 0.000000000000000000, 1.000000000000000000 ) ) ;
#6465 = AXIS2_PLACEMENT_3D ( 'NONE', #1523, #7903, #2145 ) ;
#6466 = VERTEX_POINT ( 'NONE', #4236 ) ;
#6467 = CARTESIAN_POINT ( 'NONE',  ( 49.94812488057642241, 82.72218486298730511, 0.7721950313462304649 ) ) ;
#6468 = VERTEX_POINT ( 'NONE', #6766 ) ;
#6469 = VERTEX_POINT ( 'NONE', #1075 ) ;
#6470 = VECTOR ( 'NONE', #4029, 1000.000000000000000 ) ;
#6471 = ORIENTED_EDGE ( 'NONE', *, *, #2167, .T. ) ;
#6472 = CIRCLE ( 'NONE', #1850, 4.999999999999993783 ) ;
#6473 = VERTEX_POINT ( 'NONE', #3617 ) ;
#6474 = CARTESIAN_POINT ( 'NONE',  ( 38.58716857408421674, 108.0000000000001421, 4.165101599090693094E-14 ) ) ;
#6475 = DIRECTION ( 'NONE',  ( -0.8191520442889896891, 1.003171929053522158E-16, 0.5735764363510490460 ) ) ;
#6476 = DIRECTION ( 'NONE',  ( 0.9284655864536451864, -0.3714184362296634734, -2.775557561562891351E-17 ) ) ;
#6477 = AXIS2_PLACEMENT_3D ( 'NONE', #6948, #3802, #4460 ) ;
#6478 = ADVANCED_FACE ( 'NONE', ( #2982 ), #8041, .T. ) ;
#6479 = VECTOR ( 'NONE', #4942, 1000.000000000000000 ) ;
#6480 = EDGE_CURVE ( 'NONE', #5864, #5731, #6271, .T. ) ;
#6481 = AXIS2_PLACEMENT_3D ( 'NONE', #7454, #466, #5595 ) ;
#6482 = CIRCLE ( 'NONE', #5071, 1.610000000000000098 ) ;
#6483 = EDGE_CURVE ( 'NONE', #2115, #3432, #7404, .T. ) ;
#6484 = ORIENTED_EDGE ( 'NONE', *, *, #549, .T. ) ;
#6485 = B_SPLINE_CURVE_WITH_KNOTS ( 'NONE', 3,
 ( #5426, #7947, #2266, #4677, #1518, #4054, #4343, #1685, #4395, #3639, #427, #6829, #6081, #7986, #470, #6873, #1865, #3005, #1817, #4885, #2474, #2343, #7457, #8155, #1774 ),
 .UNSPECIFIED., .F., .F.,
 ( 4, 2, 2, 1, 2, 2, 2, 2, 2, 2, 2, 2, 4 ),
 ( 0.02188532927265061934, 0.02325358088725200043, 0.02393770669455269270, 0.02462183250185338151, 0.02530595830915407379, 0.02599008411645476260, 0.02735833573105614369, 0.02804246153835683597, 0.02872658734565752478, 0.03009483896025890587, 0.03077896476755959815, 0.03146309057486028349, 0.03283134218946166805 ),
 .UNSPECIFIED. ) ;
#6486 = ORIENTED_EDGE ( 'NONE', *, *, #5702, .F. ) ;
#6487 = ORIENTED_EDGE ( 'NONE', *, *, #7763, .F. ) ;
#6488 = AXIS2_PLACEMENT_3D ( 'NONE', #6418, #3230, #5184 ) ;
#6489 = FACE_OUTER_BOUND ( 'NONE', #4619, .T. ) ;
#6490 = DIRECTION ( 'NONE',  ( -0.000000000000000000, 1.000000000000000000, 1.224646799147353207E-16 ) ) ;
#6491 = AXIS2_PLACEMENT_3D ( 'NONE', #5382, #1481, #2841 ) ;
#6492 = LINE ( 'NONE', #4589, #7130 ) ;
#6493 = SURFACE_STYLE_FILL_AREA ( #5110 ) ;
#6494 = AXIS2_PLACEMENT_3D ( 'NONE', #1781, #5607, #2442 ) ;
#6495 = VECTOR ( 'NONE', #7835, 999.9999999999998863 ) ;
#6496 = AXIS2_PLACEMENT_3D ( 'NONE', #6092, #4104, #394 ) ;
#6497 = FACE_OUTER_BOUND ( 'NONE', #16, .T. ) ;
#6498 = EDGE_CURVE ( 'NONE', #5094, #157, #371, .T. ) ;
#6499 = DIRECTION ( 'NONE',  ( -1.000000000000000000, 0.000000000000000000, 0.000000000000000000 ) ) ;
#6500 = CARTESIAN_POINT ( 'NONE',  ( -39.99999999999999289, -39.99999999999999289, 10.00000000000000000 ) ) ;
#6501 = CIRCLE ( 'NONE', #5428, 2.649999999999999467 ) ;
#6502 = DIRECTION ( 'NONE',  ( 1.000000000000000000, 1.502586498047605218E-16, -1.412205397084881070E-17 ) ) ;
#6503 = CARTESIAN_POINT ( 'NONE',  ( -49.94597403161980509, 87.32391958025807810, 0.6195456578941136438 ) ) ;
#6504 = EDGE_CURVE ( 'NONE', #821, #1158, #1831, .T. ) ;
#6505 = ORIENTED_EDGE ( 'NONE', *, *, #620, .T. ) ;
#6506 = CARTESIAN_POINT ( 'NONE',  ( 0.000000000000000000, 0.8865213383406687075, -1.535500000000000975 ) ) ;
#6507 = CARTESIAN_POINT ( 'NONE',  ( 55.00000000000000000, -8.000000000000001776, -4.499999999999986677 ) ) ;
#6508 = EDGE_CURVE ( 'NONE', #6596, #7269, #3023, .T. ) ;
#6509 = FACE_OUTER_BOUND ( 'NONE', #3662, .T. ) ;
#6510 = CARTESIAN_POINT ( 'NONE',  ( 50.00000000000000000, 9.534646258076108189E-15, 56.64999999999997726 ) ) ;
#6511 = ORIENTED_EDGE ( 'NONE', *, *, #3875, .T. ) ;
#6512 = CARTESIAN_POINT ( 'NONE',  ( 49.94550380033331294, 82.66312158132835464, -0.6298752594702436980 ) ) ;
#6513 = ORIENTED_EDGE ( 'NONE', *, *, #4461, .F. ) ;
#6514 = ORIENTED_EDGE ( 'NONE', *, *, #1598, .T. ) ;
#6515 = FACE_OUTER_BOUND ( 'NONE', #4737, .T. ) ;
#6516 = EDGE_CURVE ( 'NONE', #2553, #3093, #3031, .T. ) ;
#6517 = FACE_BOUND ( 'NONE', #5643, .T. ) ;
#6518 = CARTESIAN_POINT ( 'NONE',  ( -30.00000000000000355, -29.99999999999999289, 10.00000000000000000 ) ) ;
#6519 = CONTEXT_DEPENDENT_SHAPE_REPRESENTATION ( #1375, #3054 ) ;
#6520 = VECTOR ( 'NONE', #6545, 1000.000000000000114 ) ;
#6521 = ORIENTED_EDGE ( 'NONE', *, *, #920, .T. ) ;
#6522 = ORIENTED_EDGE ( 'NONE', *, *, #329, .T. ) ;
#6523 = VERTEX_POINT ( 'NONE', #1881 ) ;
#6524 = CARTESIAN_POINT ( 'NONE',  ( 2.000000000000000000, 1.773042676681340968, -2.276824562219559311E-15 ) ) ;
#6525 = CARTESIAN_POINT ( 'NONE',  ( -41.99999999999998579, 85.23667541621748001, 2.400000000000024336 ) ) ;
#6526 = DIRECTION ( 'NONE',  ( 1.000000000000000000, 0.000000000000000000, 0.000000000000000000 ) ) ;
#6527 =( NAMED_UNIT ( * ) PLANE_ANGLE_UNIT ( ) SI_UNIT ( $, .RADIAN. ) );
#6528 = DIRECTION ( 'NONE',  ( -1.000000000000000000, -0.000000000000000000, -0.000000000000000000 ) ) ;
#6529 = FACE_OUTER_BOUND ( 'NONE', #5508, .T. ) ;
#6530 = CARTESIAN_POINT ( 'NONE',  ( 2.500000000000002220, 0.000000000000000000, 0.000000000000000000 ) ) ;
#6531 = CARTESIAN_POINT ( 'NONE',  ( 52.00000000000000000, 7.999999999999996447, 11.99999999999998934 ) ) ;
#6532 = FACE_OUTER_BOUND ( 'NONE', #4344, .T. ) ;
#6533 = DIRECTION ( 'NONE',  ( -1.000000000000000000, 0.000000000000000000, 0.000000000000000000 ) ) ;
#6534 = PRESENTATION_LAYER_ASSIGNMENT (  '', '', ( #6950 ) ) ;
#6535 = DIRECTION ( 'NONE',  ( 0.000000000000000000, 0.000000000000000000, 1.000000000000000000 ) ) ;
#6536 = ADVANCED_FACE ( 'NONE', ( #6311 ), #7680, .F. ) ;
#6537 = ADVANCED_FACE ( 'NONE', ( #1114, #4280 ), #4448, .T. ) ;
#6538 = VERTEX_POINT ( 'NONE', #613 ) ;
#6539 = EDGE_CURVE ( 'NONE', #157, #5094, #1452, .T. ) ;
#6540 = CARTESIAN_POINT ( 'NONE',  ( 55.00000000000000000, 8.000000000000000000, -4.499999999999986677 ) ) ;
#6541 = PLANE ( 'NONE',  #6363 ) ;
#6542 = CARTESIAN_POINT ( 'NONE',  ( 1.599999999999980993, 42.68016229225776925, 4.000000000000000000 ) ) ;
#6543 = CARTESIAN_POINT ( 'NONE',  ( -41.97904239022134476, 83.67335008385822448, 2.000000000000043521 ) ) ;
#6544 = DIRECTION ( 'NONE',  ( 1.000000000000000000, 0.000000000000000000, 0.000000000000000000 ) ) ;
#6545 = DIRECTION ( 'NONE',  ( 0.000000000000000000, 0.4999999999999991673, -0.8660254037844391517 ) ) ;
#6546 = ORIENTED_EDGE ( 'NONE', *, *, #7157, .T. ) ;
#6547 = DIRECTION ( 'NONE',  ( 0.000000000000000000, -0.5000000000000008882, -0.8660254037844380415 ) ) ;
#6548 = UNCERTAINTY_MEASURE_WITH_UNIT (LENGTH_MEASURE( 1.000000000000000082E-05 ), #2424, 'distance_accuracy_value', 'NONE');
#6549 = CIRCLE ( 'NONE', #2971, 4.999999999999993783 ) ;
#6550 = ORIENTED_EDGE ( 'NONE', *, *, #2178, .T. ) ;
#6551 = VERTEX_POINT ( 'NONE', #1246 ) ;
#6552 = CARTESIAN_POINT ( 'NONE',  ( 0.3263565795980698514, -4.430380094434307914, -2.451519936624962703 ) ) ;
#6553 = DIRECTION ( 'NONE',  ( 1.000000000000000000, 0.000000000000000000, -0.000000000000000000 ) ) ;
#6554 = DIRECTION ( 'NONE',  ( 0.000000000000000000, 0.000000000000000000, -1.000000000000000000 ) ) ;
#6555 = PRODUCT_CONTEXT ( 'NONE', #3234, 'mechanical' ) ;
#6556 = ORIENTED_EDGE ( 'NONE', *, *, #7062, .T. ) ;
#6557 = ADVANCED_FACE ( 'NONE', ( #7562 ), #3209, .F. ) ;
#6558 = EDGE_LOOP ( 'NONE', ( #2502, #5017, #2090, #2281 ) ) ;
#6559 = ORIENTED_EDGE ( 'NONE', *, *, #6839, .T. ) ;
#6560 = DIRECTION ( 'NONE',  ( 1.412205397084881070E-17, -2.775557561562891967E-17, -1.000000000000000000 ) ) ;
#6561 = CARTESIAN_POINT ( 'NONE',  ( 1.300000000000000044, -0.7390083445627200209, 1.280000000000001137 ) ) ;
#6562 = CARTESIAN_POINT ( 'NONE',  ( 0.000000000000000000, -0.8865213383406690406, 1.535500000000000975 ) ) ;
#6563 = PRESENTATION_STYLE_ASSIGNMENT (( #2680 ) ) ;
#6564 = FACE_OUTER_BOUND ( 'NONE', #7204, .T. ) ;
#6565 = CARTESIAN_POINT ( 'NONE',  ( 55.00000000000000000, 10.00000000000000000, 17.64999999999999858 ) ) ;
#6566 = CIRCLE ( 'NONE', #6182, 1.535500000000000087 ) ;
#6567 =( LENGTH_UNIT ( ) NAMED_UNIT ( * ) SI_UNIT ( .MILLI., .METRE. ) );
#6568 = CARTESIAN_POINT ( 'NONE',  ( 3.999999999999999112, 0.000000000000000000, 0.000000000000000000 ) ) ;
#6569 = ADVANCED_FACE ( 'NONE', ( #5573 ), #3748, .F. ) ;
#6570 = DIRECTION ( 'NONE',  ( -0.000000000000000000, -1.000000000000000000, -0.000000000000000000 ) ) ;
#6571 = EDGE_CURVE ( 'NONE', #1899, #2969, #4752, .T. ) ;
#6572 = VECTOR ( 'NONE', #5199, 1000.000000000000000 ) ;
#6573 = ORIENTED_EDGE ( 'NONE', *, *, #8123, .F. ) ;
#6574 = VECTOR ( 'NONE', #5898, 1000.000000000000000 ) ;
#6575 = DIRECTION ( 'NONE',  ( 1.000000000000000000, 0.000000000000000000, 0.000000000000000000 ) ) ;
#6576 = FACE_OUTER_BOUND ( 'NONE', #709, .T. ) ;
#6577 = CARTESIAN_POINT ( 'NONE',  ( 42.00000000000003553, 85.00000000000049738, 2.399999999999971934 ) ) ;
#6578 = LINE ( 'NONE', #7057, #102 ) ;
#6579 = DIRECTION ( 'NONE',  ( 1.000000000000000000, -0.000000000000000000, 0.000000000000000000 ) ) ;
#6580 = DIRECTION ( 'NONE',  ( 0.000000000000000000, 0.000000000000000000, 1.000000000000000000 ) ) ;
#6581 = CARTESIAN_POINT ( 'NONE',  ( 24.00000000000000000, 1.610000000000000098, 0.000000000000000000 ) ) ;
#6582 = ORIENTED_EDGE ( 'NONE', *, *, #5689, .T. ) ;
#6583 = DIRECTION ( 'NONE',  ( 0.000000000000000000, 0.000000000000000000, 1.000000000000000000 ) ) ;
#6584 = VERTEX_POINT ( 'NONE', #6973 ) ;
#6585 = ORIENTED_EDGE ( 'NONE', *, *, #5910, .F. ) ;
#6586 = CIRCLE ( 'NONE', #3550, 2.149999999999992362 ) ;
#6587 = DIRECTION ( 'NONE',  ( -0.000000000000000000, -0.000000000000000000, -1.000000000000000000 ) ) ;
#6588 = DIRECTION ( 'NONE',  ( 0.000000000000000000, 1.000000000000000000, -1.287488025362403787E-15 ) ) ;
#6589 = VECTOR ( 'NONE', #7547, 1000.000000000000000 ) ;
#6590 = DIRECTION ( 'NONE',  ( 0.000000000000000000, -0.000000000000000000, 1.000000000000000000 ) ) ;
#6591 = EDGE_CURVE ( 'NONE', #4032, #1235, #1288, .T. ) ;
#6592 = CYLINDRICAL_SURFACE ( 'NONE', #6073, 3.500000000000000000 ) ;
#6593 = CIRCLE ( 'NONE', #760, 1.649999999999998579 ) ;
#6594 = EDGE_CURVE ( 'NONE', #3182, #6902, #7476, .T. ) ;
#6595 = CIRCLE ( 'NONE', #3025, 1.280000000000000027 ) ;
#6596 = VERTEX_POINT ( 'NONE', #1151 ) ;
#6597 = VERTEX_POINT ( 'NONE', #1753 ) ;
#6598 = ORIENTED_EDGE ( 'NONE', *, *, #1918, .F. ) ;
#6599 = EDGE_CURVE ( 'NONE', #5903, #1297, #1791, .T. ) ;
#6600 = CARTESIAN_POINT ( 'NONE',  ( 1.274374112546295138E-14, 85.00000000000017053, 2.000000000000043521 ) ) ;
#6601 = VECTOR ( 'NONE', #6026, 1000.000000000000000 ) ;
#6602 = APPLICATION_CONTEXT ( 'automotive_design' ) ;
#6603 = CYLINDRICAL_SURFACE ( 'NONE', #3989, 1.649999999999991696 ) ;
#6604 = DIRECTION ( 'NONE',  ( 1.412205397084881070E-17, -2.775557561562891967E-17, -1.000000000000000000 ) ) ;
#6605 = CLOSED_SHELL ( 'NONE', ( #5022, #6034, #4661, #2259, #17, #634, #3496, #5104, #5783, #3313 ) ) ;
#6606 = AXIS2_PLACEMENT_3D ( 'NONE', #446, #5450, #4152 ) ;
#6607 = CIRCLE ( 'NONE', #7405, 4.000000000000000888 ) ;
#6608 =( NAMED_UNIT ( * ) SI_UNIT ( $, .STERADIAN. ) SOLID_ANGLE_UNIT ( ) );
#6609 = CONICAL_SURFACE ( 'NONE', #901, 2.055000000000000160, 0.7853981633974717047 ) ;
#6610 = DIRECTION ( 'NONE',  ( 1.412205397084881070E-17, -2.775557561562891967E-17, -1.000000000000000000 ) ) ;
#6611 = CONICAL_SURFACE ( 'NONE', #1178, 1.250000000000001110, 1.029744258676655200 ) ;
#6612 = CARTESIAN_POINT ( 'NONE',  ( 3.000000000000000888, 35.09008114612887397, 4.000000000000000000 ) ) ;
#6613 = DIRECTION ( 'NONE',  ( 0.000000000000000000, 0.000000000000000000, 1.000000000000000000 ) ) ;
#6614 = AXIS2_PLACEMENT_3D ( 'NONE', #2688, #2534, #6392 ) ;
#6615 = SURFACE_STYLE_FILL_AREA ( #1551 ) ;
#6616 = VECTOR ( 'NONE', #1803, 1000.000000000000114 ) ;
#6617 = PLANE ( 'NONE',  #7958 ) ;
#6618 = CONICAL_SURFACE ( 'NONE', #526, 1.610000000000000098, 0.7853981633974647103 ) ;
#6619 = CARTESIAN_POINT ( 'NONE',  ( 4.000000000000000000, 0.000000000000000000, 0.000000000000000000 ) ) ;
#6620 = EDGE_LOOP ( 'NONE', ( #403, #4726 ) ) ;
#6621 = ORIENTED_EDGE ( 'NONE', *, *, #7207, .T. ) ;
#6622 = DIRECTION ( 'NONE',  ( 0.000000000000000000, -0.5000000000000009992, -0.8660254037844380415 ) ) ;
#6623 = AXIS2_PLACEMENT_3D ( 'NONE', #2893, #5966, #346 ) ;
#6624 = CARTESIAN_POINT ( 'NONE',  ( 0.000000000000000000, 0.000000000000000000, 10.00000000000000000 ) ) ;
#6625 = LINE ( 'NONE', #2768, #1700 ) ;
#6626 = CARTESIAN_POINT ( 'NONE',  ( 34.99999999999997868, 30.00000000000001421, 10.00000000000000000 ) ) ;
#6627 = CARTESIAN_POINT ( 'NONE',  ( 0.000000000000000000, 0.000000000000000000, 18.00000000000000355 ) ) ;
#6628 = EDGE_CURVE ( 'NONE', #5311, #3297, #3703, .T. ) ;
#6629 = DIRECTION ( 'NONE',  ( -1.000000000000000000, -0.000000000000000000, -0.000000000000000000 ) ) ;
#6630 = EDGE_CURVE ( 'NONE', #471, #5793, #6432, .T. ) ;
#6631 = DIRECTION ( 'NONE',  ( 0.000000000000000000, 0.000000000000000000, 1.000000000000000000 ) ) ;
#6632 = VERTEX_POINT ( 'NONE', #184 ) ;
#6633 = LINE ( 'NONE', #5487, #1956 ) ;
#6634 = ORIENTED_EDGE ( 'NONE', *, *, #5351, .T. ) ;
#6635 = EDGE_LOOP ( 'NONE', ( #7074, #4899, #682, #6138, #6406, #793 ) ) ;
#6636 = AXIS2_PLACEMENT_3D ( 'NONE', #3902, #5736, #7006 ) ;
#6637 = DIRECTION ( 'NONE',  ( -1.000000000000000000, 0.000000000000000000, 0.000000000000000000 ) ) ;
#6638 = DIRECTION ( 'NONE',  ( -1.412205397084881070E-17, 2.775557561562891967E-17, 1.000000000000000000 ) ) ;
#6639 = DIRECTION ( 'NONE',  ( -0.000000000000000000, -0.000000000000000000, 1.000000000000000000 ) ) ;
#6640 = DIRECTION ( 'NONE',  ( 0.000000000000000000, 0.000000000000000000, 1.000000000000000000 ) ) ;
#6641 = LINE ( 'NONE', #5453, #6740 ) ;
#6642 = SHAPE_DEFINITION_REPRESENTATION ( #1055, #2475 ) ;
#6643 = EDGE_LOOP ( 'NONE', ( #4144, #3724 ) ) ;
#6644 = ADVANCED_FACE ( 'NONE', ( #3327 ), #152, .F. ) ;
#6645 = ADVANCED_FACE ( 'NONE', ( #4532 ), #6541, .F. ) ;
#6646 = ORIENTED_EDGE ( 'NONE', *, *, #7278, .T. ) ;
#6647 = VERTEX_POINT ( 'NONE', #698 ) ;
#6648 = EDGE_CURVE ( 'NONE', #1037, #4948, #5827, .T. ) ;
#6649 = LINE ( 'NONE', #2091, #5053 ) ;
#6650 = CARTESIAN_POINT ( 'NONE',  ( 9.020562060468115204E-14, -7.000000000000000000, 7.999999999999977796 ) ) ;
#6651 = DIRECTION ( 'NONE',  ( -0.000000000000000000, 0.000000000000000000, 1.000000000000000000 ) ) ;
#6652 = FILL_AREA_STYLE ('',( #1547 ) ) ;
#6653 = B_SPLINE_CURVE_WITH_KNOTS ( 'NONE', 3,
 ( #535, #6226, #8094, #3117 ),
 .UNSPECIFIED., .F., .F.,
 ( 4, 4 ),
 ( 2.380737581783742469E-07, 0.002336974151641522165 ),
 .UNSPECIFIED. ) ;
#6654 = VECTOR ( 'NONE', #7908, 1000.000000000000000 ) ;
#6655 = ORIENTED_EDGE ( 'NONE', *, *, #100, .F. ) ;
#6656 = CARTESIAN_POINT ( 'NONE',  ( -32.64999999999999858, -29.99999999999999289, 10.00000000000000000 ) ) ;
#6657 = MANIFOLD_SOLID_BREP ( 'CBORE for M5 Hex Socket Head Cap Screw2', #1707 ) ;
#6658 = VECTOR ( 'NONE', #212, 1000.000000000000000 ) ;
#6659 = CARTESIAN_POINT ( 'NONE',  ( -0.6554360035617884384, 4.240386000424038571, -0.1586754815284916187 ) ) ;
#6660 = DIRECTION ( 'NONE',  ( 1.412205397084881070E-17, -2.775557561562891967E-17, -1.000000000000000000 ) ) ;
#6661 = DIRECTION ( 'NONE',  ( -0.000000000000000000, -0.000000000000000000, -1.000000000000000000 ) ) ;
#6662 = DIRECTION ( 'NONE',  ( 1.000000000000000000, 0.000000000000000000, 0.000000000000000000 ) ) ;
#6663 = ADVANCED_FACE ( 'NONE', ( #1336 ), #811, .F. ) ;
#6664 = ORIENTED_EDGE ( 'NONE', *, *, #1420, .T. ) ;
#6665 = ORIENTED_EDGE ( 'NONE', *, *, #6820, .F. ) ;
#6666 = DIRECTION ( 'NONE',  ( 1.000000000000000000, 0.000000000000000000, 0.000000000000000000 ) ) ;
#6667 = DIRECTION ( 'NONE',  ( -1.000000000000000000, -0.000000000000000000, -0.000000000000000000 ) ) ;
#6668 = LINE ( 'NONE', #6542, #7398 ) ;
#6669 = CARTESIAN_POINT ( 'NONE',  ( -41.94437084781007030, 87.16184554312398802, 1.050092974071262786 ) ) ;
#6670 = CARTESIAN_POINT ( 'NONE',  ( -3.000000000000000888, 45.09008114612887397, 4.000000000000000000 ) ) ;
#6671 = CARTESIAN_POINT ( 'NONE',  ( -54.99999999999990052, 10.00000000000000000, 15.49999999999877254 ) ) ;
#6672 = EDGE_CURVE ( 'NONE', #7241, #5220, #3436, .T. ) ;
#6673 = DIRECTION ( 'NONE',  ( 0.000000000000000000, 0.000000000000000000, 1.000000000000000000 ) ) ;
#6674 = EDGE_LOOP ( 'NONE', ( #1457, #6484, #3888, #2049 ) ) ;
#6675 = DIRECTION ( 'NONE',  ( -1.000000000000000000, 0.000000000000000000, 0.000000000000000000 ) ) ;
#6676 = ORIENTED_EDGE ( 'NONE', *, *, #5703, .F. ) ;
#6677 = ORIENTED_EDGE ( 'NONE', *, *, #2192, .T. ) ;
#6678 = COLOUR_RGB ( '', 0.09019608, 0.27058824, 0.51372549) ;
#6679 = DIRECTION ( 'NONE',  ( 0.000000000000000000, -0.5000000000000013323, -0.8660254037844378194 ) ) ;
#6680 = FACE_OUTER_BOUND ( 'NONE', #783, .T. ) ;
#6681 = CARTESIAN_POINT ( 'NONE',  ( 19.61000000000001720, 0.000000000000000000, 0.000000000000000000 ) ) ;
#6682 = CARTESIAN_POINT ( 'NONE',  ( -6.063573224773413095, 3.505086101364692563, 8.025480671672065469 ) ) ;
#6683 = CARTESIAN_POINT ( 'NONE',  ( 40.00000000000000711, 40.00000000000000711, 0.000000000000000000 ) ) ;
#6684 = APPLICATION_PROTOCOL_DEFINITION ( 'draft international standard', 'automotive_design', 1998, #767 ) ;
#6685 = ADVANCED_FACE ( 'NONE', ( #67 ), #2006, .F. ) ;
#6686 = MANIFOLD_SOLID_BREP ( 'M4 Clearance Hole2', #3428 ) ;
#6687 = ORIENTED_EDGE ( 'NONE', *, *, #2840, .F. ) ;
#6688 = EDGE_CURVE ( 'NONE', #4663, #7783, #2507, .T. ) ;
#6689 = ORIENTED_EDGE ( 'NONE', *, *, #6594, .T. ) ;
#6690 = ORIENTED_EDGE ( 'NONE', *, *, #596, .T. ) ;
#6691 = CIRCLE ( 'NONE', #6429, 3.500000000000000000 ) ;
#6692 = DIRECTION ( 'NONE',  ( 1.000000000000000000, 0.000000000000000000, 0.000000000000000000 ) ) ;
#6693 = DIRECTION ( 'NONE',  ( -1.000000000000000000, 0.000000000000000000, 1.112002228190260397E-17 ) ) ;
#6694 = FACE_OUTER_BOUND ( 'NONE', #1799, .T. ) ;
#6695 = SURFACE_STYLE_FILL_AREA ( #6652 ) ;
#6696 = EDGE_LOOP ( 'NONE', ( #5031, #6369, #7103, #119 ) ) ;
#6697 = CYLINDRICAL_SURFACE ( 'NONE', #2079, 1.250000000000001110 ) ;
#6698 = DIRECTION ( 'NONE',  ( 0.000000000000000000, 0.000000000000000000, -1.000000000000000000 ) ) ;
#6699 =( REPRESENTATION_RELATIONSHIP ('NONE','NONE', #3916, #499 ) REPRESENTATION_RELATIONSHIP_WITH_TRANSFORMATION ( #7388 )SHAPE_REPRESENTATION_RELATIONSHIP( ) );
#6700 = CARTESIAN_POINT ( 'NONE',  ( 1.300000000000000044, 0.7390083445627224634, 1.279999999999999138 ) ) ;
#6701 = FILL_AREA_STYLE ('',( #4211 ) ) ;
#6702 = DIRECTION ( 'NONE',  ( 0.000000000000000000, 0.000000000000000000, -1.000000000000000000 ) ) ;
#6703 = CARTESIAN_POINT ( 'NONE',  ( 32.64999999999997726, 30.00000000000001421, 4.599999999999997868 ) ) ;
#6704 = ORIENTED_EDGE ( 'NONE', *, *, #2665, .T. ) ;
#6705 = VERTEX_POINT ( 'NONE', #933 ) ;
#6706 = VECTOR ( 'NONE', #7757, 1000.000000000000000 ) ;
#6707 = ADVANCED_FACE ( 'NONE', ( #390 ), #5390, .F. ) ;
#6708 = FACE_OUTER_BOUND ( 'NONE', #2550, .T. ) ;
#6709 = FACE_OUTER_BOUND ( 'NONE', #7187, .T. ) ;
#6710 = FACE_OUTER_BOUND ( 'NONE', #2809, .T. ) ;
#6711 = CARTESIAN_POINT ( 'NONE',  ( -59.99999999999999289, 85.00000000000045475, 2.399999999999971489 ) ) ;
#6712 = CARTESIAN_POINT ( 'NONE',  ( 23.61000000000001364, 0.000000000000000000, 2.000000000000000444 ) ) ;
#6713 = PLANE ( 'NONE',  #5955 ) ;
#6714 = ORIENTED_EDGE ( 'NONE', *, *, #2563, .F. ) ;
#6715 = AXIS2_PLACEMENT_3D ( 'NONE', #7245, #391, #218 ) ;
#6716 = FACE_OUTER_BOUND ( 'NONE', #6784, .T. ) ;
#6717 = VECTOR ( 'NONE', #571, 1000.000000000000000 ) ;
#6718 = EDGE_LOOP ( 'NONE', ( #5750, #6285, #7739, #2498, #829 ) ) ;
#6719 = ORIENTED_EDGE ( 'NONE', *, *, #2446, .F. ) ;
#6720 = CARTESIAN_POINT ( 'NONE',  ( -4.000000000000000000, 2.309401076758531346, -2.342734410091827701 ) ) ;
#6721 = FACE_OUTER_BOUND ( 'NONE', #861, .T. ) ;
#6722 = DIRECTION ( 'NONE',  ( -1.000000000000000000, -0.000000000000000000, -0.000000000000000000 ) ) ;
#6723 = DIRECTION ( 'NONE',  ( 0.000000000000000000, 0.000000000000000000, 1.000000000000000000 ) ) ;
#6724 = DIRECTION ( 'NONE',  ( 0.000000000000000000, 0.000000000000000000, 1.000000000000000000 ) ) ;
#6725 = ORIENTED_EDGE ( 'NONE', *, *, #6298, .F. ) ;
#6726 = VERTEX_POINT ( 'NONE', #343 ) ;
#6727 = EDGE_LOOP ( 'NONE', ( #7215, #3114, #269 ) ) ;
#6728 = CARTESIAN_POINT ( 'NONE',  ( -38.58716857408418122, 108.0000000000001990, -4.999999999999976907 ) ) ;
#6729 = EDGE_CURVE ( 'NONE', #7794, #1727, #1611, .T. ) ;
#6730 = CARTESIAN_POINT ( 'NONE',  ( 0.000000000000000000, 0.000000000000000000, 0.000000000000000000 ) ) ;
#6731 = DIRECTION ( 'NONE',  ( 1.000000000000000000, 0.000000000000000000, 0.000000000000000000 ) ) ;
#6732 = ADVANCED_FACE ( 'NONE', ( #6576 ), #7001, .F. ) ;
#6733 = CONICAL_SURFACE ( 'NONE', #3167, 1.250000000000001110, 1.029744258676655200 ) ;
#6734 =( NAMED_UNIT ( * ) SI_UNIT ( $, .STERADIAN. ) SOLID_ANGLE_UNIT ( ) );
#6735 = EDGE_CURVE ( 'NONE', #4315, #4688, #5416, .T. ) ;
#6736 = AXIS2_PLACEMENT_3D ( 'NONE', #25, #6342, #3314 ) ;
#6737 = ORIENTED_EDGE ( 'NONE', *, *, #6057, .F. ) ;
#6738 = PLANE ( 'NONE',  #77 ) ;
#6739 = ORIENTED_EDGE ( 'NONE', *, *, #2862, .F. ) ;
#6740 = VECTOR ( 'NONE', #4073, 1000.000000000000000 ) ;
#6741 = AXIS2_PLACEMENT_3D ( 'NONE', #3065, #8082, #3011 ) ;
#6742 = AXIS2_PLACEMENT_3D ( 'NONE', #3699, #1290, #6274 ) ;
#6743 = LINE ( 'NONE', #512, #3859 ) ;
#6744 = DIRECTION ( 'NONE',  ( 0.000000000000000000, 0.000000000000000000, -1.000000000000000000 ) ) ;
#6745 = FILL_AREA_STYLE_COLOUR ( '', #3903 ) ;
#6746 = DIRECTION ( 'NONE',  ( -0.000000000000000000, -0.000000000000000000, 1.000000000000000000 ) ) ;
#6747 = VECTOR ( 'NONE', #6845, 1000.000000000000114 ) ;
#6748 = DIRECTION ( 'NONE',  ( 0.000000000000000000, 0.8660254037844380415, -0.5000000000000011102 ) ) ;
#6749 = CIRCLE ( 'NONE', #5704, 2.000000000000000888 ) ;
#6750 = ORIENTED_EDGE ( 'NONE', *, *, #7367, .T. ) ;
#6751 = ORIENTED_EDGE ( 'NONE', *, *, #5635, .F. ) ;
#6752 = VECTOR ( 'NONE', #1215, 1000.000000000000227 ) ;
#6753 = VECTOR ( 'NONE', #5944, 1000.000000000000000 ) ;
#6754 = CARTESIAN_POINT ( 'NONE',  ( -41.93122696811912675, 87.40254376044632068, -0.06342023833167842461 ) ) ;
#6755 = DIRECTION ( 'NONE',  ( -0.000000000000000000, -0.000000000000000000, 1.000000000000000000 ) ) ;
#6756 = CARTESIAN_POINT ( 'NONE',  ( -49.94236411077203996, 82.59994436935571116, -0.1557065084607691663 ) ) ;
#6757 = CIRCLE ( 'NONE', #1596, 0.2000000000000000944 ) ;
#6758 = DIRECTION ( 'NONE',  ( 0.000000000000000000, -0.4999999999999993339, 0.8660254037844389297 ) ) ;
#6759 = VERTEX_POINT ( 'NONE', #3390 ) ;
#6760 = LINE ( 'NONE', #4273, #7379 ) ;
#6761 = VERTEX_POINT ( 'NONE', #217 ) ;
#6762 = CIRCLE ( 'NONE', #6623, 4.999999999999997335 ) ;
#6763 = EDGE_LOOP ( 'NONE', ( #1543, #7817, #5246 ) ) ;
#6764 = ADVANCED_FACE ( 'NONE', ( #7332 ), #3434, .T. ) ;
#6765 = DIRECTION ( 'NONE',  ( -0.000000000000000000, 1.000000000000000000, -0.000000000000000000 ) ) ;
#6766 = CARTESIAN_POINT ( 'NONE',  ( -2.000000000000009770, 3.464101615137749057, 0.000000000000000000 ) ) ;
#6767 = DIRECTION ( 'NONE',  ( 0.000000000000000000, 0.000000000000000000, 1.000000000000000000 ) ) ;
#6768 = CARTESIAN_POINT ( 'NONE',  ( -3.505070609393837522, 6.076439379008851560, 8.008416788275647846 ) ) ;
#6769 = AXIS2_PLACEMENT_3D ( 'NONE', #4516, #5680, #3775 ) ;
#6770 = ITEM_DEFINED_TRANSFORMATION ( 'NONE', 'NONE', #4971,  #1587 ) ;
#6771 = APPLICATION_CONTEXT ( 'automotive_design' ) ;
#6772 = AXIS2_PLACEMENT_3D ( 'NONE', #1242, #6928, #3826 ) ;
#6773 = ORIENTED_EDGE ( 'NONE', *, *, #7098, .F. ) ;
#6774 = ORIENTED_EDGE ( 'NONE', *, *, #2178, .F. ) ;
#6775 = EDGE_CURVE ( 'NONE', #7382, #5247, #4490, .T. ) ;
#6776 = ORIENTED_EDGE ( 'NONE', *, *, #3007, .F. ) ;
#6777 = DIRECTION ( 'NONE',  ( -0.000000000000000000, -0.000000000000000000, 1.000000000000000000 ) ) ;
#6778 = DIRECTION ( 'NONE',  ( -1.000000000000000000, -2.775557561562890365E-16, 1.734723475976806478E-17 ) ) ;
#6779 = UNCERTAINTY_MEASURE_WITH_UNIT (LENGTH_MEASURE( 1.000000000000000082E-05 ), #599, 'distance_accuracy_value', 'NONE');
#6780 =( NAMED_UNIT ( * ) PLANE_ANGLE_UNIT ( ) SI_UNIT ( $, .RADIAN. ) );
#6781 = ORIENTED_EDGE ( 'NONE', *, *, #4302, .F. ) ;
#6782 = CARTESIAN_POINT ( 'NONE',  ( 40.00000000000000711, -39.99999999999999289, 10.00000000000000000 ) ) ;
#6783 = EDGE_LOOP ( 'NONE', ( #5157, #2292 ) ) ;
#6784 = EDGE_LOOP ( 'NONE', ( #5705, #1686, #2586, #7150, #2579, #6377 ) ) ;
#6785 = ADVANCED_FACE ( 'NONE', ( #5963, #6708 ), #1014, .T. ) ;
#6786 = CYLINDRICAL_SURFACE ( 'NONE', #3977, 2.149999999999995470 ) ;
#6787 = CARTESIAN_POINT ( 'NONE',  ( -41.93694480353852327, 82.69900792083214469, 0.6941923800780730458 ) ) ;
#6788 = SURFACE_STYLE_USAGE ( .BOTH. , #3547 ) ;
#6789 = DIRECTION ( 'NONE',  ( 0.000000000000000000, 0.000000000000000000, -1.000000000000000000 ) ) ;
#6790 = CIRCLE ( 'NONE', #3233, 42.00000000000002132 ) ;
#6791 = VERTEX_POINT ( 'NONE', #2222 ) ;
#6792 = EDGE_LOOP ( 'NONE', ( #7595, #8038, #717, #2466 ) ) ;
#6793 = DIRECTION ( 'NONE',  ( -1.000000000000000000, -0.000000000000000000, -0.000000000000000000 ) ) ;
#6794 = CARTESIAN_POINT ( 'NONE',  ( 60.00000000000004263, 85.00000000000051159, -1.387778780781445676E-14 ) ) ;
#6795 = DIRECTION ( 'NONE',  ( 1.000000000000000000, 0.000000000000000000, 0.000000000000000000 ) ) ;
#6796 = FACE_OUTER_BOUND ( 'NONE', #6783, .T. ) ;
#6797 = DIRECTION ( 'NONE',  ( 1.000000000000000000, 0.000000000000000000, -0.000000000000000000 ) ) ;
#6798 = EDGE_CURVE ( 'NONE', #1855, #6979, #7133, .T. ) ;
#6799 = DIRECTION ( 'NONE',  ( 0.8571673007021118895, 2.194743421410583551E-16, -0.5150380749100549327 ) ) ;
#6800 = EDGE_CURVE ( 'NONE', #683, #366, #6341, .T. ) ;
#6801 = ORIENTED_EDGE ( 'NONE', *, *, #7233, .T. ) ;
#6802 = ORIENTED_EDGE ( 'NONE', *, *, #7163, .T. ) ;
#6803 = DIRECTION ( 'NONE',  ( -0.000000000000000000, -0.000000000000000000, 1.000000000000000000 ) ) ;
#6804 = DIRECTION ( 'NONE',  ( -1.000000000000000000, 0.000000000000000000, 0.000000000000000000 ) ) ;
#6805 = DIRECTION ( 'NONE',  ( 0.000000000000000000, -0.5000000000000009992, -0.8660254037844380415 ) ) ;
#6806 = DIRECTION ( 'NONE',  ( 0.000000000000000000, 0.4999999999999993339, -0.8660254037844390407 ) ) ;
#6807 = CARTESIAN_POINT ( 'NONE',  ( -1.588057467863390526, 6.821288780608425917, 8.001713687856982560 ) ) ;
#6808 = CARTESIAN_POINT ( 'NONE',  ( 49.98564705169091837, 86.20508806345003450, -2.081488237565429777 ) ) ;
#6809 = ITEM_DEFINED_TRANSFORMATION ( 'NONE', 'NONE', #3502,  #1587 ) ;
#6810 = ORIENTED_EDGE ( 'NONE', *, *, #4978, .T. ) ;
#6811 = ORIENTED_EDGE ( 'NONE', *, *, #1635, .T. ) ;
#6812 = ORIENTED_EDGE ( 'NONE', *, *, #2070, .T. ) ;
#6813 = ORIENTED_EDGE ( 'NONE', *, *, #222, .F. ) ;
#6814 = DIRECTION ( 'NONE',  ( 1.412205397084881070E-17, -2.775557561562891967E-17, -1.000000000000000000 ) ) ;
#6816 = EDGE_CURVE ( 'NONE', #6819, #7658, #4083, .T. ) ;
#6815 = CARTESIAN_POINT ( 'NONE',  ( 4.440873302168275031E-15, 38.99999999999999289, 0.7510757737844847570 ) ) ;
#6817 = CARTESIAN_POINT ( 'NONE',  ( 9.020562075079396891E-14, 10.00000000000000000, 729.2499999999977263 ) ) ;
#6818 = EDGE_CURVE ( 'NONE', #191, #4437, #4742, .T. ) ;
#6819 = VERTEX_POINT ( 'NONE', #2309 ) ;
#6820 = EDGE_CURVE ( 'NONE', #6988, #7449, #4845, .T. ) ;
#6821 = DIRECTION ( 'NONE',  ( -1.000000000000000000, 0.000000000000000000, 0.000000000000000000 ) ) ;
#6822 = VERTEX_POINT ( 'NONE', #975 ) ;
#6823 = AXIS2_PLACEMENT_3D ( 'NONE', #7010, #4531, #1333 ) ;
#6824 = ORIENTED_EDGE ( 'NONE', *, *, #6800, .F. ) ;
#6825 = LINE ( 'NONE', #4297, #5427 ) ;
#6826 = CARTESIAN_POINT ( 'NONE',  ( 41.08716857408421674, 108.0000000000001421, 4.165101599090693094E-14 ) ) ;
#6827 = PRODUCT_DEFINITION_SHAPE ( 'NONE', 'NONE',  #7571 ) ;
#6828 = CARTESIAN_POINT ( 'NONE',  ( -6.632365264926793458, -2.250456567307095757, 8.030492030296132455 ) ) ;
#6829 = CARTESIAN_POINT ( 'NONE',  ( 5.273939683826339930, 4.625367979329794821, 8.019210142024537191 ) ) ;
#6830 = ORIENTED_EDGE ( 'NONE', *, *, #5611, .T. ) ;
#6831 = ORIENTED_EDGE ( 'NONE', *, *, #5976, .T. ) ;
#6832 = ADVANCED_BREP_SHAPE_REPRESENTATION ( '', ( #6657, #1587 ), #517 ) ;
#6833 = DIRECTION ( 'NONE',  ( 0.000000000000000000, 0.000000000000000000, 1.000000000000000000 ) ) ;
#6834 = LINE ( 'NONE', #5685, #652 ) ;
#6835 = DIRECTION ( 'NONE',  ( 1.412205397084881070E-17, -2.775557561562891967E-17, -1.000000000000000000 ) ) ;
#6836 = EDGE_CURVE ( 'NONE', #366, #683, #3419, .T. ) ;
#6837 = CARTESIAN_POINT ( 'NONE',  ( 4.000000000000003553, 2.309401076758480720, -2.700000000000000178 ) ) ;
#6838 = CARTESIAN_POINT ( 'NONE',  ( 58.00000000000000000, 8.000000000000000000, -8.000000000000000000 ) ) ;
#6839 = EDGE_CURVE ( 'NONE', #4324, #1776, #7260, .T. ) ;
#6840 = DIRECTION ( 'NONE',  ( -1.000000000000000000, 0.000000000000000000, 0.000000000000000000 ) ) ;
#6841 = VERTEX_POINT ( 'NONE', #3064 ) ;
#6842 = ORIENTED_EDGE ( 'NONE', *, *, #2698, .F. ) ;
#6843 = DIRECTION ( 'NONE',  ( -1.000000000000000000, 0.000000000000000000, 1.032573497605241731E-17 ) ) ;
#6844 = PLANE ( 'NONE',  #6082 ) ;
#6845 = DIRECTION ( 'NONE',  ( -0.7071067811865355823, 8.659560562355079537E-17, -0.7071067811865595631 ) ) ;
#6846 = CARTESIAN_POINT ( 'NONE',  ( 4.200000000000001954, 0.000000000000000000, 0.000000000000000000 ) ) ;
#6847 = CARTESIAN_POINT ( 'NONE',  ( 1.284259550325887758E-14, 85.00000000000005684, -5.000000000000004441 ) ) ;
#6848 = CARTESIAN_POINT ( 'NONE',  ( 49.95352446852413664, 87.15616155047293034, 1.065671633021458842 ) ) ;
#6849 = AXIS2_PLACEMENT_3D ( 'NONE', #4145, #2233, #4770 ) ;
#6850 = ORIENTED_EDGE ( 'NONE', *, *, #1858, .T. ) ;
#6851 = ORIENTED_EDGE ( 'NONE', *, *, #4013, .T. ) ;
#6852 = ORIENTED_EDGE ( 'NONE', *, *, #6255, .F. ) ;
#6853 = VERTEX_POINT ( 'NONE', #1062 ) ;
#6854 = EDGE_CURVE ( 'NONE', #1738, #2405, #5163, .T. ) ;
#6855 = CARTESIAN_POINT ( 'NONE',  ( 1.270137496355039850E-14, 85.00000000000011369, 5.000000000000046185 ) ) ;
#6856 = DIRECTION ( 'NONE',  ( 0.000000000000000000, -1.000000000000000000, 0.000000000000000000 ) ) ;
#6857 = ADVANCED_FACE ( 'NONE', ( #4438 ), #565, .F. ) ;
#6858 = CARTESIAN_POINT ( 'NONE',  ( 2.500000000000002220, -1.178949249685218970, -2.041999999999998483 ) ) ;
#6859 = CARTESIAN_POINT ( 'NONE',  ( 0.000000000000000000, 0.000000000000000000, 0.000000000000000000 ) ) ;
#6860 = EDGE_LOOP ( 'NONE', ( #3654, #5101, #7314, #3486 ) ) ;
#6861 = CARTESIAN_POINT ( 'NONE',  ( 40.00000000000000711, -39.99999999999999289, 0.000000000000000000 ) ) ;
#6862 = ORIENTED_EDGE ( 'NONE', *, *, #5815, .T. ) ;
#6863 = ADVANCED_FACE ( 'NONE', ( #6132 ), #8050, .T. ) ;
#6864 = ORIENTED_EDGE ( 'NONE', *, *, #7203, .F. ) ;
#6865 = EDGE_CURVE ( 'NONE', #2944, #3913, #6260, .T. ) ;
#6866 = CIRCLE ( 'NONE', #4216, 3.299999999999999822 ) ;
#6867 = CARTESIAN_POINT ( 'NONE',  ( 41.99796613401628775, 85.46972184547207974, 2.365094516100901156 ) ) ;
#6868 = CARTESIAN_POINT ( 'NONE',  ( -41.93506701445380003, 82.66515142059692778, -0.5699281247693004371 ) ) ;
#6869 = DIRECTION ( 'NONE',  ( 1.000000000000000000, 0.000000000000000000, 0.000000000000000000 ) ) ;
#6870 =( NAMED_UNIT ( * ) PLANE_ANGLE_UNIT ( ) SI_UNIT ( $, .RADIAN. ) );
#6871 = LINE ( 'NONE', #5513, #680 ) ;
#6872 = VECTOR ( 'NONE', #5606, 1000.000000000000000 ) ;
#6873 = CARTESIAN_POINT ( 'NONE',  ( 4.077904861489376032, 5.694132991774995212, 8.011503056869331729 ) ) ;
#6874 = AXIS2_PLACEMENT_3D ( 'NONE', #2224, #6043, #8031 ) ;
#6875 = CIRCLE ( 'NONE', #3698, 4.250000000000000000 ) ;
#6876 = VERTEX_POINT ( 'NONE', #8124 ) ;
#6877 = ORIENTED_EDGE ( 'NONE', *, *, #5049, .F. ) ;
#6878 = DIRECTION ( 'NONE',  ( -1.000000000000000000, -0.000000000000000000, -0.000000000000000000 ) ) ;
#6879 = CARTESIAN_POINT ( 'NONE',  ( 0.000000000000000000, -1.178949249685218970, -2.041999999999998483 ) ) ;
#6880 = DIRECTION ( 'NONE',  ( 0.000000000000000000, 0.000000000000000000, -1.000000000000000000 ) ) ;
#6881 = VECTOR ( 'NONE', #2872, 1000.000000000000000 ) ;
#6882 = FACE_BOUND ( 'NONE', #1257, .T. ) ;
#6883 = AXIS2_PLACEMENT_3D ( 'NONE', #691, #3238, #2611 ) ;
#6884 = DIRECTION ( 'NONE',  ( 0.000000000000000000, 1.000000000000000000, -1.224646799147353207E-16 ) ) ;
#6885 = AXIS2_PLACEMENT_3D ( 'NONE', #8040, #356, #2282 ) ;
#6886 = PLANE ( 'NONE',  #618 ) ;
#6887 = ORIENTED_EDGE ( 'NONE', *, *, #6936, .T. ) ;
#6888 = AXIS2_PLACEMENT_3D ( 'NONE', #5985, #4124, #7190 ) ;
#6889 = DIRECTION ( 'NONE',  ( 0.000000000000000000, 0.000000000000000000, 1.000000000000000000 ) ) ;
#6890 = CARTESIAN_POINT ( 'NONE',  ( 1.300000000000000044, 1.478016689125442484, -1.626303258728256651E-15 ) ) ;
#6891 = DIRECTION ( 'NONE',  ( 1.000000000000000000, 0.000000000000000000, 0.000000000000000000 ) ) ;
#6892 = DIRECTION ( 'NONE',  ( -1.000000000000000000, 0.000000000000000000, 0.000000000000000000 ) ) ;
#6893 = CARTESIAN_POINT ( 'NONE',  ( -32.64999999999999858, -29.99999999999999289, 1.734723475976807094E-15 ) ) ;
#6894 = CARTESIAN_POINT ( 'NONE',  ( 49.96357426530715884, 86.91018610273397371, -1.461418215542109600 ) ) ;
#6895 = AXIS2_PLACEMENT_3D ( 'NONE', #8087, #2314, #437 ) ;
#6896 = ITEM_DEFINED_TRANSFORMATION ( 'NONE', 'NONE', #298,  #1587 ) ;
#6897 = VERTEX_POINT ( 'NONE', #6303 ) ;
#6898 = AXIS2_PLACEMENT_3D ( 'NONE', #1636, #4163, #6692 ) ;
#6899 = CIRCLE ( 'NONE', #6491, 1.250000000000001110 ) ;
#6900 = CIRCLE ( 'NONE', #791, 1.599999999999986766 ) ;
#6901 = MANIFOLD_SOLID_BREP ( 'Hex', #2761 ) ;
#6902 = VERTEX_POINT ( 'NONE', #5557 ) ;
#6903 = ORIENTED_EDGE ( 'NONE', *, *, #942, .T. ) ;
#6904 = EDGE_LOOP ( 'NONE', ( #6573, #1355, #4492, #214, #6991 ) ) ;
#6905 = PRODUCT_DEFINITION_SHAPE ( 'NONE', 'NONE',  #8222 ) ;
#6906 = CARTESIAN_POINT ( 'NONE',  ( 52.00000000000000000, -8.000000000000003553, 11.99999999999998934 ) ) ;
#6907 = DIRECTION ( 'NONE',  ( 0.000000000000000000, 0.000000000000000000, 1.000000000000000000 ) ) ;
#6908 = VECTOR ( 'NONE', #1064, 1000.000000000000000 ) ;
#6909 = FACE_OUTER_BOUND ( 'NONE', #7393, .T. ) ;
#6910 = FILL_AREA_STYLE_COLOUR ( '', #1788 ) ;
#6911 = ORIENTED_EDGE ( 'NONE', *, *, #7847, .F. ) ;
#6912 = CARTESIAN_POINT ( 'NONE',  ( 49.96368263234901974, 83.09261300472560663, -1.465190138156190924 ) ) ;
#6913 = EDGE_CURVE ( 'NONE', #5387, #1263, #3152, .T. ) ;
#6914 = ORIENTED_EDGE ( 'NONE', *, *, #3102, .T. ) ;
#6915 = EDGE_CURVE ( 'NONE', #683, #7269, #4307, .T. ) ;
#6916 = EDGE_CURVE ( 'NONE', #3364, #2129, #2294, .T. ) ;
#6917 = EDGE_LOOP ( 'NONE', ( #2429, #5074, #2219, #1749 ) ) ;
#6918 = MANIFOLD_SOLID_BREP ( 'M4 Clearance Hole1', #7797 ) ;
#6919 = DIRECTION ( 'NONE',  ( 0.000000000000000000, 0.000000000000000000, -1.000000000000000000 ) ) ;
#6920 = CARTESIAN_POINT ( 'NONE',  ( -41.95042219981622367, 82.95369115198531063, 1.280157006458463531 ) ) ;
#6921 = CARTESIAN_POINT ( 'NONE',  ( -54.99999999999990052, -8.000000000000001776, 15.49999999999877254 ) ) ;
#6922 = CARTESIAN_POINT ( 'NONE',  ( 5.200000000000020606, 3.061616997868392016E-16, -2.500000000000007994 ) ) ;
#6923 = ORIENTED_EDGE ( 'NONE', *, *, #5156, .F. ) ;
#6924 = VERTEX_POINT ( 'NONE', #2099 ) ;
#6925 = CARTESIAN_POINT ( 'NONE',  ( 1.300000000000000044, -0.7390083445627225744, -1.279999999999999138 ) ) ;
#6926 = DIRECTION ( 'NONE',  ( -1.412205397084881070E-17, 2.775557561562891967E-17, 1.000000000000000000 ) ) ;
#6927 = FACE_OUTER_BOUND ( 'NONE', #5757, .T. ) ;
#6928 = DIRECTION ( 'NONE',  ( 0.000000000000000000, -1.000000000000000000, 0.000000000000000000 ) ) ;
#6929 = CARTESIAN_POINT ( 'NONE',  ( 60.00000000000000711, 9.534646258076108189E-15, 56.64999999999997016 ) ) ;
#6930 = CIRCLE ( 'NONE', #7186, 2.099999999999999645 ) ;
#6931 = EDGE_CURVE ( 'NONE', #4508, #2164, #756, .T. ) ;
#6932 = ORIENTED_EDGE ( 'NONE', *, *, #6189, .F. ) ;
#6933 = DIRECTION ( 'NONE',  ( 1.000000000000000000, 0.000000000000000000, 0.000000000000000000 ) ) ;
#6934 = CARTESIAN_POINT ( 'NONE',  ( -30.00000000000000355, -29.99999999999999289, 4.599999999999997868 ) ) ;
#6935 = FACE_BOUND ( 'NONE', #1931, .T. ) ;
#6936 = EDGE_CURVE ( 'NONE', #6468, #3337, #2097, .T. ) ;
#6937 = VECTOR ( 'NONE', #2522, 1000.000000000000000 ) ;
#6938 = DIRECTION ( 'NONE',  ( 1.000000000000000000, 2.775557561562890365E-16, -1.734723475976806478E-17 ) ) ;
#6939 = CARTESIAN_POINT ( 'NONE',  ( 49.99926415638497446, 85.31227754079901615, 2.384817760534212017 ) ) ;
#6940 = ORIENTED_EDGE ( 'NONE', *, *, #5445, .T. ) ;
#6941 = ORIENTED_EDGE ( 'NONE', *, *, #197, .T. ) ;
#6942 = CARTESIAN_POINT ( 'NONE',  ( 41.98525237464914284, 83.86985196153031552, 2.130344599767619584 ) ) ;
#6943 = VECTOR ( 'NONE', #2349, 1000.000000000000000 ) ;
#6944 = ORIENTED_EDGE ( 'NONE', *, *, #5878, .T. ) ;
#6945 = ORIENTED_EDGE ( 'NONE', *, *, #6234, .F. ) ;
#6946 = DIRECTION ( 'NONE',  ( -1.000000000000000000, 0.000000000000000000, 0.000000000000000000 ) ) ;
#6947 = CARTESIAN_POINT ( 'NONE',  ( -58.00000000000006395, 7.999999999999996447, 11.99999999999998934 ) ) ;
#6948 = CARTESIAN_POINT ( 'NONE',  ( 24.00000000000000000, 0.000000000000000000, 0.000000000000000000 ) ) ;
#6949 = EDGE_CURVE ( 'NONE', #493, #7254, #3171, .T. ) ;
#6950 = STYLED_ITEM ( 'NONE', ( #2519 ), #5182 ) ;
#6951 = VERTEX_POINT ( 'NONE', #5732 ) ;
#6952 = DIRECTION ( 'NONE',  ( -1.000000000000000000, 0.000000000000000000, 0.000000000000000000 ) ) ;
#6953 = EDGE_CURVE ( 'NONE', #8184, #7025, #1696, .T. ) ;
#6954 = ORIENTED_EDGE ( 'NONE', *, *, #3583, .F. ) ;
#6955 = VERTEX_POINT ( 'NONE', #3981 ) ;
#6956 = DIRECTION ( 'NONE',  ( 0.000000000000000000, -0.5000000000000009992, -0.8660254037844380415 ) ) ;
#6957 = CARTESIAN_POINT ( 'NONE',  ( 41.93354940223066762, 87.36172033103325418, -0.4455622145788336597 ) ) ;
#6958 = DIRECTION ( 'NONE',  ( -1.000000000000000000, -0.000000000000000000, -0.000000000000000000 ) ) ;
#6959 = SHAPE_REPRESENTATION_RELATIONSHIP ( 'NONE' , 'NONE' ,  #6987, #293 ) ;
#6960 = CARTESIAN_POINT ( 'NONE',  ( 30.00000000000001066, -29.99999999999997868, 1.734723475976807094E-15 ) ) ;
#6961 = ORIENTED_EDGE ( 'NONE', *, *, #1582, .F. ) ;
#6962 = CARTESIAN_POINT ( 'NONE',  ( 2.000000000000000000, 0.8865213383406717051, 1.535499999999998533 ) ) ;
#6963 = DIRECTION ( 'NONE',  ( 0.000000000000000000, 0.000000000000000000, -1.000000000000000000 ) ) ;
#6964 = DIRECTION ( 'NONE',  ( 1.000000000000000000, 0.000000000000000000, -1.112002228190260397E-17 ) ) ;
#6965 = CARTESIAN_POINT ( 'NONE',  ( -52.00000000000006395, 7.999999999999996447, 11.99999999999998934 ) ) ;
#6966 = EDGE_CURVE ( 'NONE', #931, #5489, #7632, .T. ) ;
#6967 = CARTESIAN_POINT ( 'NONE',  ( 0.000000000000000000, 0.000000000000000000, 0.000000000000000000 ) ) ;
#6968 = CARTESIAN_POINT ( 'NONE',  ( -49.98564705169090416, 86.20508806344973607, 2.081488237565525701 ) ) ;
#6969 = PRODUCT_DEFINITION_SHAPE ( 'NONE', 'NONE',  #8209 ) ;
#6970 = ADVANCED_FACE ( 'NONE', ( #7002 ), #1949, .F. ) ;
#6971 = ORIENTED_EDGE ( 'NONE', *, *, #1500, .T. ) ;
#6972 = CARTESIAN_POINT ( 'NONE',  ( -52.00000000000006395, -8.000000000000003553, 11.99999999999998934 ) ) ;
#6973 = CARTESIAN_POINT ( 'NONE',  ( 50.00000000000000000, 10.00000000000000000, 0.000000000000000000 ) ) ;
#6974 = DIRECTION ( 'NONE',  ( 1.000000000000000000, 0.000000000000000000, 0.000000000000000000 ) ) ;
#6975 = B_SPLINE_CURVE_WITH_KNOTS ( 'NONE', 3,
 ( #3212, #7643, #2491, #5037, #1962, #7564 ),
 .UNSPECIFIED., .F., .F.,
 ( 4, 2, 4 ),
 ( 0.006456566858647395761, 0.007625406818786647362, 0.008794246778925899830 ),
 .UNSPECIFIED. ) ;
#6976 = CARTESIAN_POINT ( 'NONE',  ( 2.000000000000000000, 0.8865213383406687075, -1.535500000000000975 ) ) ;
#6977 = LINE ( 'NONE', #1291, #7921 ) ;
#6978 = ORIENTED_EDGE ( 'NONE', *, *, #1784, .T. ) ;
#6979 = VERTEX_POINT ( 'NONE', #4559 ) ;
#6980 = LINE ( 'NONE', #5046, #5442 ) ;
#6981 = EDGE_LOOP ( 'NONE', ( #1308, #7685, #6852, #6122 ) ) ;
#6982 = ORIENTED_EDGE ( 'NONE', *, *, #386, .T. ) ;
#6983 = CIRCLE ( 'NONE', #6039, 2.650000000000003020 ) ;
#6984 = DIRECTION ( 'NONE',  ( 1.000000000000000000, 0.000000000000000000, 0.000000000000000000 ) ) ;
#6985 = DIRECTION ( 'NONE',  ( -0.5000000000000061062, 0.000000000000000000, 0.8660254037844351549 ) ) ;
#6986 = CARTESIAN_POINT ( 'NONE',  ( -39.99999999999999289, -39.99999999999999289, 10.00000000000000000 ) ) ;
#6987 = SHAPE_REPRESENTATION ( 'V_bar', ( #1587 ), #1923 ) ;
#6988 = VERTEX_POINT ( 'NONE', #6962 ) ;
#6989 = CIRCLE ( 'NONE', #3837, 1.610000000000000098 ) ;
#6990 = AXIS2_PLACEMENT_3D ( 'NONE', #6173, #8129, #5565 ) ;
#6991 = ORIENTED_EDGE ( 'NONE', *, *, #4472, .T. ) ;
#6992 = EDGE_LOOP ( 'NONE', ( #5417, #6505 ) ) ;
#6993 = EDGE_CURVE ( 'NONE', #4662, #2397, #2004, .T. ) ;
#6994 = CARTESIAN_POINT ( 'NONE',  ( 2.000000000000000000, 1.690103923579303787E-15, 1.535499999999999865 ) ) ;
#6995 = EDGE_CURVE ( 'NONE', #5386, #3008, #7713, .T. ) ;
#6996 = CARTESIAN_POINT ( 'NONE',  ( 0.000000000000000000, 1.478016689125442484, -1.626303258728256651E-15 ) ) ;
#6997 = FACE_OUTER_BOUND ( 'NONE', #461, .T. ) ;
#6998 = EDGE_CURVE ( 'NONE', #1966, #1132, #1278, .T. ) ;
#6999 =( LENGTH_UNIT ( ) NAMED_UNIT ( * ) SI_UNIT ( .MILLI., .METRE. ) );
#7000 = VERTEX_POINT ( 'NONE', #7778 ) ;
#7001 = TOROIDAL_SURFACE ( 'NONE', #6465, 2.700000000000000622, 0.2000000000000000111 ) ;
#7002 = FACE_OUTER_BOUND ( 'NONE', #3367, .T. ) ;
#7003 = DIRECTION ( 'NONE',  ( 1.412205397084881070E-17, -2.775557561562891967E-17, -1.000000000000000000 ) ) ;
#7004 = CARTESIAN_POINT ( 'NONE',  ( 3.000000000000002665, 3.367778697655221012E-16, -2.750000000000000000 ) ) ;
#7005 = DIRECTION ( 'NONE',  ( -1.000000000000000000, -0.000000000000000000, -0.000000000000000000 ) ) ;
#7006 = DIRECTION ( 'NONE',  ( 0.000000000000000000, 0.000000000000000000, 1.000000000000000000 ) ) ;
#7007 = DIRECTION ( 'NONE',  ( 0.000000000000000000, 1.000000000000000000, 0.000000000000000000 ) ) ;
#7008 = EDGE_CURVE ( 'NONE', #5475, #7622, #5848, .T. ) ;
#7009 = ORIENTED_EDGE ( 'NONE', *, *, #4527, .T. ) ;
#7010 = CARTESIAN_POINT ( 'NONE',  ( 1.270137496355039850E-14, 85.00000000000011369, 5.000000000000046185 ) ) ;
#7011 = VECTOR ( 'NONE', #5099, 1000.000000000000000 ) ;
#7012 = CLOSED_SHELL ( 'NONE', ( #3610, #1214, #5084, #5916, #1095, #7724, #1980, #96, #1079, #3322, #7122, #7252, #3264, #7543, #4412, #3895, #3890, #2321, #4151, #2496, #2274, #24, #839, #6663, #5358, #7409, #4536 ) ) ;
#7013 = DIRECTION ( 'NONE',  ( 0.000000000000000000, -1.000000000000000000, 0.000000000000000000 ) ) ;
#7014 = VECTOR ( 'NONE', #7347, 1000.000000000000000 ) ;
#7015 = AXIS2_PLACEMENT_3D ( 'NONE', #5822, #3338, #2705 ) ;
#7016 = FACE_OUTER_BOUND ( 'NONE', #73, .T. ) ;
#7017 = CARTESIAN_POINT ( 'NONE',  ( 2.000000000000027089, 3.464101615137739731, 0.000000000000000000 ) ) ;
#7018 = ORIENTED_EDGE ( 'NONE', *, *, #187, .F. ) ;
#7019 = AXIS2_PLACEMENT_3D ( 'NONE', #3244, #3359, #7719 ) ;
#7020 = EDGE_CURVE ( 'NONE', #2205, #4530, #5438, .T. ) ;
#7021 = AXIS2_PLACEMENT_3D ( 'NONE', #6453, #757, #3312 ) ;
#7022 = ORIENTED_EDGE ( 'NONE', *, *, #1924, .T. ) ;
#7023 = AXIS2_PLACEMENT_3D ( 'NONE', #5605, #650, #4401 ) ;
#7024 = DIRECTION ( 'NONE',  ( -1.000000000000000000, -0.000000000000000000, -0.000000000000000000 ) ) ;
#7025 = VERTEX_POINT ( 'NONE', #2686 ) ;
#7026 = ORIENTED_EDGE ( 'NONE', *, *, #5528, .T. ) ;
#7027 = VECTOR ( 'NONE', #396, 1000.000000000000000 ) ;
#7028 = LINE ( 'NONE', #4543, #2640 ) ;
#7029 = CARTESIAN_POINT ( 'NONE',  ( -31.74999999999995737, 0.000000000000000000, 0.000000000000000000 ) ) ;
#7030 = CARTESIAN_POINT ( 'NONE',  ( 30.00000000000000000, 0.000000000000000000, -6.938893903907228378E-15 ) ) ;
#7031 = VECTOR ( 'NONE', #4429, 1000.000000000000114 ) ;
#7032 = DIRECTION ( 'NONE',  ( -1.000000000000000000, -5.833327817117372205E-17, -1.734723475976807094E-18 ) ) ;
#7033 = VECTOR ( 'NONE', #1644, 1000.000000000000000 ) ;
#7034 = AXIS2_PLACEMENT_3D ( 'NONE', #2313, #6629, #937 ) ;
#7035 = ORIENTED_EDGE ( 'NONE', *, *, #593, .T. ) ;
#7036 = ORIENTED_EDGE ( 'NONE', *, *, #338, .T. ) ;
#7037 = EDGE_CURVE ( 'NONE', #5106, #7290, #6424, .T. ) ;
#7038 = VERTEX_POINT ( 'NONE', #5150 ) ;
#7039 = CIRCLE ( 'NONE', #2010, 2.149999999999992362 ) ;
#7040 = CARTESIAN_POINT ( 'NONE',  ( -27.34999999999999076, 30.00000000000000711, 4.599999999999997868 ) ) ;
#7041 = CARTESIAN_POINT ( 'NONE',  ( 41.93162583688302902, 87.39562999375550589, -0.1928873818979062182 ) ) ;
#7042 = DIRECTION ( 'NONE',  ( 1.000000000000000000, 0.000000000000000000, 0.000000000000000000 ) ) ;
#7043 = MECHANICAL_DESIGN_GEOMETRIC_PRESENTATION_REPRESENTATION (  '', ( #3061 ), #5454 ) ;
#7044 = CARTESIAN_POINT ( 'NONE',  ( -2.252029883699507629, -6.631804555459141604, 8.003482568582050760 ) ) ;
#7045 = ADVANCED_FACE ( 'NONE', ( #7667 ), #4594, .T. ) ;
#7046 = AXIS2_PLACEMENT_3D ( 'NONE', #2175, #4709, #7238 ) ;
#7047 = CARTESIAN_POINT ( 'NONE',  ( 0.000000000000000000, 0.000000000000000000, 18.00000000000000355 ) ) ;
#7048 = CARTESIAN_POINT ( 'NONE',  ( 39.83716857408421674, 108.0000000000001421, 4.163336342344337027E-14 ) ) ;
#7049 = DIRECTION ( 'NONE',  ( 0.000000000000000000, 0.000000000000000000, 1.000000000000000000 ) ) ;
#7050 = CARTESIAN_POINT ( 'NONE',  ( -30.00000000000000355, -29.99999999999999289, 4.599999999999997868 ) ) ;
#7051 = CYLINDRICAL_SURFACE ( 'NONE', #1745, 4.999999999999993783 ) ;
#7052 = CARTESIAN_POINT ( 'NONE',  ( -49.95662654559777849, 87.08399340104890030, 1.200635520122923072 ) ) ;
#7053 = ORIENTED_EDGE ( 'NONE', *, *, #3836, .T. ) ;
#7054 = CARTESIAN_POINT ( 'NONE',  ( -3.345653888883672433, 2.687187980154694955, -0.1391502195351393689 ) ) ;
#7055 = DIRECTION ( 'NONE',  ( -1.000000000000000000, 0.000000000000000000, 1.412205397084881070E-17 ) ) ;
#7056 = DIRECTION ( 'NONE',  ( 0.000000000000000000, 1.000000000000000000, -1.103561164596346103E-15 ) ) ;
#7057 = CARTESIAN_POINT ( 'NONE',  ( 60.00000000000000711, -10.00000000000000000, 60.00000000000000000 ) ) ;
#7058 = SURFACE_STYLE_FILL_AREA ( #1491 ) ;
#7059 = AXIS2_PLACEMENT_3D ( 'NONE', #1882, #6892, #1207 ) ;
#7060 = VERTEX_POINT ( 'NONE', #804 ) ;
#7061 = ADVANCED_FACE ( 'NONE', ( #3350 ), #5880, .T. ) ;
#7062 = EDGE_CURVE ( 'NONE', #3249, #397, #3580, .T. ) ;
#7063 = ORIENTED_EDGE ( 'NONE', *, *, #2966, .F. ) ;
#7064 = CARTESIAN_POINT ( 'NONE',  ( -4.000000000000000000, -0.3902508023145542793, -2.700000000000001066 ) ) ;
#7065 = ORIENTED_EDGE ( 'NONE', *, *, #7233, .F. ) ;
#7066 = AXIS2_PLACEMENT_3D ( 'NONE', #4301, #8117, #2435 ) ;
#7067 = ORIENTED_EDGE ( 'NONE', *, *, #3911, .F. ) ;
#7068 = CARTESIAN_POINT ( 'NONE',  ( 39.83716857408421674, 108.0000000000001990, -4.999999999999976907 ) ) ;
#7069 = DIRECTION ( 'NONE',  ( -0.000000000000000000, -0.000000000000000000, 1.000000000000000000 ) ) ;
#7070 = DIRECTION ( 'NONE',  ( -1.000000000000000000, 0.000000000000000000, 1.412205397084881070E-17 ) ) ;
#7071 = DIRECTION ( 'NONE',  ( 0.9965007563543568647, 6.113200401986782768E-17, -0.08358374593899633997 ) ) ;
#7072 = ORIENTED_EDGE ( 'NONE', *, *, #5660, .F. ) ;
#7073 = AXIS2_PLACEMENT_3D ( 'NONE', #1480, #1602, #5879 ) ;
#7074 = ORIENTED_EDGE ( 'NONE', *, *, #7308, .T. ) ;
#7075 = VERTEX_POINT ( 'NONE', #7165 ) ;
#7076 = VERTEX_POINT ( 'NONE', #2264 ) ;
#7077 = EDGE_CURVE ( 'NONE', #7241, #6897, #2173, .T. ) ;
#7078 = DIRECTION ( 'NONE',  ( 0.000000000000000000, -0.5000000000000009992, -0.8660254037844380415 ) ) ;
#7079 = CARTESIAN_POINT ( 'NONE',  ( 41.98843075541680037, 85.99227196424216402, -2.189015531278163174 ) ) ;
#7080 = DIRECTION ( 'NONE',  ( -0.000000000000000000, -0.000000000000000000, 1.000000000000000000 ) ) ;
#7081 = COLOUR_RGB ( '', 0.66274510, 0.83137255, 0.94901961) ;
#7082 = ADVANCED_FACE ( 'NONE', ( #296 ), #2758, .F. ) ;
#7083 = CARTESIAN_POINT ( 'NONE',  ( -2.650000000000006128, 3.245314017740489413E-16, 20.00000000000000355 ) ) ;
#7084 = CARTESIAN_POINT ( 'NONE',  ( 0.000000000000000000, 0.000000000000000000, 0.000000000000000000 ) ) ;
#7085 = DIRECTION ( 'NONE',  ( 0.000000000000000000, 0.000000000000000000, -1.000000000000000000 ) ) ;
#7086 = DIRECTION ( 'NONE',  ( 0.000000000000000000, 1.000000000000000000, -1.224646799147353207E-16 ) ) ;
#7087 = PRODUCT_DEFINITION_FORMATION_WITH_SPECIFIED_SOURCE ( 'ANY', '', #5585, .NOT_KNOWN. ) ;
#7088 = CARTESIAN_POINT ( 'NONE',  ( 0.000000000000000000, 0.000000000000000000, -2.674599999999998978 ) ) ;
#7089 = CARTESIAN_POINT ( 'NONE',  ( -49.99422766321047362, 85.77334557296515527, -2.277359159638559394 ) ) ;
#7090 = VECTOR ( 'NONE', #4154, 1000.000000000000000 ) ;
#7091 = ORIENTED_EDGE ( 'NONE', *, *, #8017, .F. ) ;
#7092 = FACE_OUTER_BOUND ( 'NONE', #6299, .T. ) ;
#7093 = EDGE_CURVE ( 'NONE', #992, #4428, #380, .T. ) ;
#7094 = DIRECTION ( 'NONE',  ( 1.000000000000000000, 0.000000000000000000, 0.000000000000000000 ) ) ;
#7095 = PLANE ( 'NONE',  #6329 ) ;
#7096 = EDGE_CURVE ( 'NONE', #5129, #7219, #6899, .T. ) ;
#7097 = CARTESIAN_POINT ( 'NONE',  ( -31.74999999999995737, 0.000000000000000000, 3.500000000000000000 ) ) ;
#7098 = EDGE_CURVE ( 'NONE', #5311, #7330, #378, .T. ) ;
#7099 = CARTESIAN_POINT ( 'NONE',  ( -49.99422363137627201, 84.22622254513437667, 2.277283319317688015 ) ) ;
#7100 = EDGE_LOOP ( 'NONE', ( #5622, #5545, #2667, #5006, #7529, #6131 ) ) ;
#7101 = CARTESIAN_POINT ( 'NONE',  ( -2.339468227445729465, -3.268109542640674547, -2.699999999999984190 ) ) ;
#7102 = ORIENTED_EDGE ( 'NONE', *, *, #5201, .F. ) ;
#7103 = ORIENTED_EDGE ( 'NONE', *, *, #2698, .T. ) ;
#7104 = VERTEX_POINT ( 'NONE', #3546 ) ;
#7105 = ORIENTED_EDGE ( 'NONE', *, *, #4592, .T. ) ;
#7106 = DIRECTION ( 'NONE',  ( 1.412205397084881070E-17, -2.775557561562891967E-17, -1.000000000000000000 ) ) ;
#7107 = CARTESIAN_POINT ( 'NONE',  ( -32.64999999999999147, 30.00000000000000711, 10.00000000000000000 ) ) ;
#7108 = APPLICATION_PROTOCOL_DEFINITION ( 'draft international standard', 'automotive_design', 1998, #2367 ) ;
#7109 = ORIENTED_EDGE ( 'NONE', *, *, #3538, .F. ) ;
#7110 = EDGE_CURVE ( 'NONE', #6466, #6897, #790, .T. ) ;
#7111 = VERTEX_POINT ( 'NONE', #5422 ) ;
#7112 = AXIS2_PLACEMENT_3D ( 'NONE', #7450, #2334, #1767 ) ;
#7113 = ORIENTED_EDGE ( 'NONE', *, *, #6915, .F. ) ;
#7114 = CYLINDRICAL_SURFACE ( 'NONE', #4637, 2.649999999999999467 ) ;
#7115 = CARTESIAN_POINT ( 'NONE',  ( 41.99756812932361072, 84.48755377607589878, -2.358409241415262425 ) ) ;
#7116 = DIRECTION ( 'NONE',  ( -0.000000000000000000, -0.000000000000000000, 1.000000000000000000 ) ) ;
#7117 = PRESENTATION_STYLE_ASSIGNMENT (( #7627 ) ) ;
#7118 = VECTOR ( 'NONE', #2582, 1000.000000000000000 ) ;
#7119 = CIRCLE ( 'NONE', #1293, 4.999999999999997335 ) ;
#7120 = CYLINDRICAL_SURFACE ( 'NONE', #3593, 1.250000000000001110 ) ;
#7121 = ADVANCED_FACE ( 'NONE', ( #333 ), #4110, .T. ) ;
#7122 = ADVANCED_FACE ( 'NONE', ( #4634 ), #1730, .T. ) ;
#7123 = DIRECTION ( 'NONE',  ( -1.000000000000000000, 0.000000000000000000, 0.000000000000000000 ) ) ;
#7124 = DIRECTION ( 'NONE',  ( -0.000000000000000000, 1.000000000000000000, 1.224646799147353207E-16 ) ) ;
#7125 = DIRECTION ( 'NONE',  ( -1.000000000000000000, 0.000000000000000000, 0.000000000000000000 ) ) ;
#7126 = FACE_OUTER_BOUND ( 'NONE', #668, .T. ) ;
#7127 = ORIENTED_EDGE ( 'NONE', *, *, #620, .F. ) ;
#7128 = LINE ( 'NONE', #2692, #1400 ) ;
#7129 = DIRECTION ( 'NONE',  ( 0.000000000000000000, 0.000000000000000000, -1.000000000000000000 ) ) ;
#7130 = VECTOR ( 'NONE', #2027, 1000.000000000000000 ) ;
#7131 = PLANE ( 'NONE',  #8197 ) ;
#7132 = LINE ( 'NONE', #4646, #99 ) ;
#7133 = CIRCLE ( 'NONE', #5029, 10.00000000000000000 ) ;
#7134 = VERTEX_POINT ( 'NONE', #4052 ) ;
#7135 = DIRECTION ( 'NONE',  ( 1.412205397084881070E-17, -2.775557561562891967E-17, -1.000000000000000000 ) ) ;
#7136 = UNCERTAINTY_MEASURE_WITH_UNIT (LENGTH_MEASURE( 1.000000000000000082E-05 ), #21, 'distance_accuracy_value', 'NONE');
#7137 = VECTOR ( 'NONE', #2161, 1000.000000000000000 ) ;
#7138 = ORIENTED_EDGE ( 'NONE', *, *, #5275, .F. ) ;
#7139 = VERTEX_POINT ( 'NONE', #6700 ) ;
#7140 = VECTOR ( 'NONE', #1950, 1000.000000000000000 ) ;
#7141 = CIRCLE ( 'NONE', #4095, 4.250000000000000000 ) ;
#7142 = ORIENTED_EDGE ( 'NONE', *, *, #6162, .F. ) ;
#7143 = FACE_OUTER_BOUND ( 'NONE', #7639, .T. ) ;
#7144 = DIRECTION ( 'NONE',  ( 1.000000000000000000, 0.000000000000000000, 0.000000000000000000 ) ) ;
#7145 = ITEM_DEFINED_TRANSFORMATION ( 'NONE', 'NONE', #7623,  #1587 ) ;
#7146 = VECTOR ( 'NONE', #4906, 1000.000000000000114 ) ;
#7147 = AXIS2_PLACEMENT_3D ( 'NONE', #2757, #1549, #2878 ) ;
#7148 = CIRCLE ( 'NONE', #7280, 2.200000000000001066 ) ;
#7149 = ADVANCED_FACE ( 'NONE', ( #2213 ), #967, .F. ) ;
#7150 = ORIENTED_EDGE ( 'NONE', *, *, #860, .F. ) ;
#7151 = ORIENTED_EDGE ( 'NONE', *, *, #3693, .T. ) ;
#7152 = ORIENTED_EDGE ( 'NONE', *, *, #6729, .F. ) ;
#7153 = CARTESIAN_POINT ( 'NONE',  ( 1.274374112546295138E-14, 85.00000000000017053, 2.000000000000043521 ) ) ;
#7154 = PLANE ( 'NONE',  #2393 ) ;
#7155 = VECTOR ( 'NONE', #5954, 1000.000000000000000 ) ;
#7156 = DIRECTION ( 'NONE',  ( 0.000000000000000000, 0.000000000000000000, -1.000000000000000000 ) ) ;
#7157 = EDGE_CURVE ( 'NONE', #6246, #5583, #4913, .T. ) ;
#7158 = SURFACE_STYLE_FILL_AREA ( #919 ) ;
#7159 = EDGE_CURVE ( 'NONE', #2122, #2164, #2879, .T. ) ;
#7160 = ADVANCED_FACE ( 'NONE', ( #1005 ), #248, .T. ) ;
#7161 = AXIS2_PLACEMENT_3D ( 'NONE', #1040, #7445, #5627 ) ;
#7162 = VECTOR ( 'NONE', #4893, 1000.000000000000000 ) ;
#7163 = EDGE_CURVE ( 'NONE', #244, #4887, #7861, .T. ) ;
#7164 = DIRECTION ( 'NONE',  ( -1.000000000000000000, -1.734723475976806848E-16, 0.000000000000000000 ) ) ;
#7165 = CARTESIAN_POINT ( 'NONE',  ( 50.00000000000004974, 85.00000000000039790, -2.399999999999999467 ) ) ;
#7166 = CARTESIAN_POINT ( 'NONE',  ( -7.502679033599690683E-14, -4.618802153517020059, -2.342734410091827701 ) ) ;
#7167 = CYLINDRICAL_SURFACE ( 'NONE', #2925, 2.399999999999985256 ) ;
#7168 = CIRCLE ( 'NONE', #5457, 4.999999999999997335 ) ;
#7169 = DIRECTION ( 'NONE',  ( -1.000000000000000000, -0.000000000000000000, -0.000000000000000000 ) ) ;
#7170 = ORIENTED_EDGE ( 'NONE', *, *, #860, .T. ) ;
#7171 = FACE_OUTER_BOUND ( 'NONE', #2088, .T. ) ;
#7172 = DIRECTION ( 'NONE',  ( 0.000000000000000000, 0.000000000000000000, -1.000000000000000000 ) ) ;
#7173 = CARTESIAN_POINT ( 'NONE',  ( -54.99999999999990052, 10.00000000000000000, 17.64999999999876934 ) ) ;
#7174 = FACE_OUTER_BOUND ( 'NONE', #1380, .T. ) ;
#7175 = CARTESIAN_POINT ( 'NONE',  ( -49.98887975752123225, 83.93556181870150112, 2.156785159512773831 ) ) ;
#7176 = EDGE_CURVE ( 'NONE', #3168, #8104, #3774, .T. ) ;
#7177 = DIRECTION ( 'NONE',  ( -0.000000000000000000, 1.000000000000000000, -0.000000000000000000 ) ) ;
#7178 = ORIENTED_EDGE ( 'NONE', *, *, #4785, .F. ) ;
#7179 = LINE ( 'NONE', #6049, #5147 ) ;
#7180 = EDGE_LOOP ( 'NONE', ( #3582, #3769 ) ) ;
#7181 = EDGE_LOOP ( 'NONE', ( #1373, #2165, #7900, #7691 ) ) ;
#7182 = DIRECTION ( 'NONE',  ( -1.000000000000000000, -0.000000000000000000, -0.000000000000000000 ) ) ;
#7183 = DIRECTION ( 'NONE',  ( -0.8571673007021125557, -1.430919794933845163E-16, -0.5150380749100536004 ) ) ;
#7184 = CARTESIAN_POINT ( 'NONE',  ( 5.860087342385653250E-15, 38.99999999999999289, 0.000000000000000000 ) ) ;
#7185 = PRODUCT_CONTEXT ( 'NONE', #6771, 'mechanical' ) ;
#7186 = AXIS2_PLACEMENT_3D ( 'NONE', #2817, #7789, #3483 ) ;
#7187 = EDGE_LOOP ( 'NONE', ( #6802, #8102, #3043 ) ) ;
#7188 = EDGE_LOOP ( 'NONE', ( #3554, #1299, #7971, #1758 ) ) ;
#7189 = VERTEX_POINT ( 'NONE', #3424 ) ;
#7190 = DIRECTION ( 'NONE',  ( 0.000000000000000000, 0.000000000000000000, 1.000000000000000000 ) ) ;
#7191 = APPLICATION_CONTEXT ( 'automotive_design' ) ;
#7192 = ADVANCED_FACE ( 'NONE', ( #4088 ), #7236, .F. ) ;
#7193 = CARTESIAN_POINT ( 'NONE',  ( 52.00000000000000711, -8.000000000000000000, -8.000000000000000000 ) ) ;
#7194 = ADVANCED_FACE ( 'NONE', ( #5597 ), #4880, .T. ) ;
#7195 = EDGE_LOOP ( 'NONE', ( #7306, #2712, #5400 ) ) ;
#7196 = DIRECTION ( 'NONE',  ( -1.000000000000000000, 0.000000000000000000, 0.000000000000000000 ) ) ;
#7197 = PRODUCT_RELATED_PRODUCT_CATEGORY ( 'part', '', ( #4839 ) ) ;
#7198 = LINE ( 'NONE', #7822, #1719 ) ;
#7199 = CARTESIAN_POINT ( 'NONE',  ( 5.930697612239895941E-15, 38.99999999999999289, -4.999999999999990230 ) ) ;
#7200 = DIRECTION ( 'NONE',  ( 1.000000000000000000, 0.000000000000000000, 0.000000000000000000 ) ) ;
#7201 = PRESENTATION_LAYER_ASSIGNMENT (  '', '', ( #1510 ) ) ;
#7202 = CARTESIAN_POINT ( 'NONE',  ( 0.000000000000000000, 0.000000000000000000, -25.03750572909317285 ) ) ;
#7203 = EDGE_CURVE ( 'NONE', #2558, #5625, #4519, .T. ) ;
#7204 = EDGE_LOOP ( 'NONE', ( #817, #421, #1162, #3806 ) ) ;
#7205 = CARTESIAN_POINT ( 'NONE',  ( 38.58716857408421674, 108.0000000000001421, 4.161571085597980959E-14 ) ) ;
#7206 = AXIS2_PLACEMENT_3D ( 'NONE', #944, #3402, #3489 ) ;
#7207 = EDGE_CURVE ( 'NONE', #4877, #973, #6292, .T. ) ;
#7208 = DIRECTION ( 'NONE',  ( 0.5000000000000067724, 0.8660254037844348218, -0.000000000000000000 ) ) ;
#7209 = CARTESIAN_POINT ( 'NONE',  ( 0.000000000000000000, 0.000000000000000000, -2.700000000000001066 ) ) ;
#7210 = AXIS2_PLACEMENT_3D ( 'NONE', #629, #3259, #2052 ) ;
#7211 = DIRECTION ( 'NONE',  ( 1.000000000000000000, -0.000000000000000000, -0.000000000000000000 ) ) ;
#7212 = CARTESIAN_POINT ( 'NONE',  ( 4.000000000000003553, 2.309401076758524685, -2.342734410091827701 ) ) ;
#7213 = LINE ( 'NONE', #1615, #4914 ) ;
#7214 = LINE ( 'NONE', #5926, #1492 ) ;
#7215 = ORIENTED_EDGE ( 'NONE', *, *, #871, .T. ) ;
#7216 = CARTESIAN_POINT ( 'NONE',  ( 2.000000000000000000, 2.253471898105738645E-15, 1.535499999999999865 ) ) ;
#7217 = AXIS2_PLACEMENT_3D ( 'NONE', #5921, #7784, #4642 ) ;
#7218 = EDGE_CURVE ( 'NONE', #2129, #3553, #7944, .T. ) ;
#7219 = VERTEX_POINT ( 'NONE', #4210 ) ;
#7220 = ORIENTED_EDGE ( 'NONE', *, *, #1898, .F. ) ;
#7221 = CARTESIAN_POINT ( 'NONE',  ( -52.00000000000006395, -8.000000000000003553, 19.99999999999998934 ) ) ;
#7222 = FACE_OUTER_BOUND ( 'NONE', #3037, .T. ) ;
#7223 = CARTESIAN_POINT ( 'NONE',  ( 0.000000000000000000, 0.000000000000000000, -2.700000000000000178 ) ) ;
#7224 = FACE_OUTER_BOUND ( 'NONE', #1542, .T. ) ;
#7225 = PRODUCT_CONTEXT ( 'NONE', #2367, 'mechanical' ) ;
#7226 = VERTEX_POINT ( 'NONE', #2471 ) ;
#7227 = EDGE_LOOP ( 'NONE', ( #5409, #6095, #7885, #7522 ) ) ;
#7228 = VERTEX_POINT ( 'NONE', #8024 ) ;
#7229 = CARTESIAN_POINT ( 'NONE',  ( 7.000000000000000000, 8.572527594031473190E-16, 10.00000000000000000 ) ) ;
#7230 = DIRECTION ( 'NONE',  ( 1.412205397084881070E-17, -2.775557561562891967E-17, -1.000000000000000000 ) ) ;
#7231 = LINE ( 'NONE', #7773, #1157 ) ;
#7232 = ADVANCED_BREP_SHAPE_REPRESENTATION ( '', ( #4069, #1587 ), #2305 ) ;
#7233 = EDGE_CURVE ( 'NONE', #2820, #5254, #6200, .T. ) ;
#7234 = EDGE_CURVE ( 'NONE', #4539, #4068, #2121, .T. ) ;
#7235 = CARTESIAN_POINT ( 'NONE',  ( -2.099999999999999645, 2.571758278209440478E-16, -0.2800830152838832965 ) ) ;
#7236 = CYLINDRICAL_SURFACE ( 'NONE', #5580, 2.649999999999995914 ) ;
#7237 = CIRCLE ( 'NONE', #2868, 1.250000000000001110 ) ;
#7238 = DIRECTION ( 'NONE',  ( 1.000000000000000000, 0.000000000000000000, 0.000000000000000000 ) ) ;
#7239 = SHAPE_REPRESENTATION ( 'lock', ( #1587 ), #3101 ) ;
#7240 = DIRECTION ( 'NONE',  ( 1.000000000000000000, 0.000000000000000000, 0.000000000000000000 ) ) ;
#7241 = VERTEX_POINT ( 'NONE', #4262 ) ;
#7242 = ORIENTED_EDGE ( 'NONE', *, *, #1854, .F. ) ;
#7243 = CARTESIAN_POINT ( 'NONE',  ( 24.00000000000000000, 0.000000000000000000, 0.000000000000000000 ) ) ;
#7244 = DIRECTION ( 'NONE',  ( 0.000000000000000000, 0.000000000000000000, 1.000000000000000000 ) ) ;
#7245 = CARTESIAN_POINT ( 'NONE',  ( 0.000000000000000000, 0.000000000000000000, -2.674599999999998978 ) ) ;
#7246 = CARTESIAN_POINT ( 'NONE',  ( -41.97224931050724450, 86.54160261602827120, 1.857416509361091039 ) ) ;
#7247 = LINE ( 'NONE', #5480, #2515 ) ;
#7248 = CARTESIAN_POINT ( 'NONE',  ( 4.200000000000001954, 0.000000000000000000, 0.000000000000000000 ) ) ;
#7249 = DIRECTION ( 'NONE',  ( -1.412205397084880761E-17, -2.775557561562891967E-17, -1.000000000000000000 ) ) ;
#7250 = EDGE_CURVE ( 'NONE', #6185, #2702, #1460, .T. ) ;
#7251 = EDGE_LOOP ( 'NONE', ( #240, #6774, #6379, #533 ) ) ;
#7252 = ADVANCED_FACE ( 'NONE', ( #2339 ), #7535, .T. ) ;
#7253 = LINE ( 'NONE', #1495, #4860 ) ;
#7254 = VERTEX_POINT ( 'NONE', #6826 ) ;
#7255 = ORIENTED_EDGE ( 'NONE', *, *, #2727, .T. ) ;
#7256 = TOROIDAL_SURFACE ( 'NONE', #2751, 4.000000000000000000, 0.2500000000000000000 ) ;
#7257 = LINE ( 'NONE', #1499, #4096 ) ;
#7258 = CARTESIAN_POINT ( 'NONE',  ( 4.000000000000003553, 0.000000000000000000, 0.000000000000000000 ) ) ;
#7259 = CYLINDRICAL_SURFACE ( 'NONE', #1624, 4.999999999999997335 ) ;
#7260 = CIRCLE ( 'NONE', #8192, 1.600000000000000311 ) ;
#7261 = CARTESIAN_POINT ( 'NONE',  ( -4.625276930412667298, 5.274027880968991333, 8.014758447098458305 ) ) ;
#7262 = FACE_OUTER_BOUND ( 'NONE', #5701, .T. ) ;
#7263 = SHAPE_DEFINITION_REPRESENTATION ( #3585, #7870 ) ;
#7264 = VECTOR ( 'NONE', #5250, 1000.000000000000114 ) ;
#7265 = VECTOR ( 'NONE', #3950, 1000.000000000000000 ) ;
#7266 = CIRCLE ( 'NONE', #4226, 0.2000000000000000944 ) ;
#7267 = ORIENTED_EDGE ( 'NONE', *, *, #1466, .T. ) ;
#7268 = EDGE_LOOP ( 'NONE', ( #5632, #283, #2080, #6714 ) ) ;
#7269 = VERTEX_POINT ( 'NONE', #424 ) ;
#7270 = DIRECTION ( 'NONE',  ( 1.412205397084881070E-17, -2.775557561562891967E-17, -1.000000000000000000 ) ) ;
#7271 = AXIS2_PLACEMENT_3D ( 'NONE', #4832, #6651, #1085 ) ;
#7272 = DIRECTION ( 'NONE',  ( 1.000000000000000000, 0.000000000000000000, 0.000000000000000000 ) ) ;
#7273 = FACE_OUTER_BOUND ( 'NONE', #1073, .T. ) ;
#7274 = VECTOR ( 'NONE', #6805, 1000.000000000000114 ) ;
#7275 = CONICAL_SURFACE ( 'NONE', #4631, 1.280000000000000027, 1.047197551196593857 ) ;
#7276 =( LENGTH_UNIT ( ) NAMED_UNIT ( * ) SI_UNIT ( .MILLI., .METRE. ) );
#7277 = VECTOR ( 'NONE', #3453, 1000.000000000000000 ) ;
#7278 = EDGE_CURVE ( 'NONE', #5862, #1769, #1002, .T. ) ;
#7279 = CIRCLE ( 'NONE', #2911, 10.00000000000000000 ) ;
#7280 = AXIS2_PLACEMENT_3D ( 'NONE', #5805, #5195, #7714 ) ;
#7281 = PLANE ( 'NONE',  #653 ) ;
#7282 = DIRECTION ( 'NONE',  ( 0.000000000000000000, 0.000000000000000000, 1.000000000000000000 ) ) ;
#7283 = VECTOR ( 'NONE', #4416, 1000.000000000000227 ) ;
#7284 = SURFACE_STYLE_FILL_AREA ( #6701 ) ;
#7285 = CONICAL_SURFACE ( 'NONE', #128, 1.249999999999998002, 1.029744258676653645 ) ;
#7286 = CARTESIAN_POINT ( 'NONE',  ( 38.58716857408421674, 108.0000000000001990, -4.999999999999976907 ) ) ;
#7287 = VECTOR ( 'NONE', #6660, 1000.000000000000000 ) ;
#7288 = STYLED_ITEM ( 'NONE', ( #5162 ), #4069 ) ;
#7289 = CARTESIAN_POINT ( 'NONE',  ( 0.000000000000000000, 0.000000000000000000, 18.00000000000000355 ) ) ;
#7290 = VERTEX_POINT ( 'NONE', #3096 ) ;
#7291 = AXIS2_PLACEMENT_3D ( 'NONE', #6518, #6443, #858 ) ;
#7292 = ORIENTED_EDGE ( 'NONE', *, *, #7093, .F. ) ;
#7293 = PLANE ( 'NONE',  #7875 ) ;
#7294 = VECTOR ( 'NONE', #5436, 1000.000000000000000 ) ;
#7295 = DIRECTION ( 'NONE',  ( -1.000000000000000000, 0.000000000000000000, -0.000000000000000000 ) ) ;
#7296 = DIRECTION ( 'NONE',  ( -0.5000000000000051070, 0.000000000000000000, 0.8660254037844355990 ) ) ;
#7297 = DIRECTION ( 'NONE',  ( -0.000000000000000000, -0.000000000000000000, -1.000000000000000000 ) ) ;
#7298 = LINE ( 'NONE', #6670, #3042 ) ;
#7299 = ADVANCED_FACE ( 'NONE', ( #3893 ), #3195, .F. ) ;
#7300 = CARTESIAN_POINT ( 'NONE',  ( -49.99923958211701347, 84.68425784446330340, -2.384302390493951762 ) ) ;
#7301 = EDGE_CURVE ( 'NONE', #6955, #2355, #6051, .T. ) ;
#7302 = CARTESIAN_POINT ( 'NONE',  ( 2.000000000000000000, 1.329782007511006281, 0.7677499999999990443 ) ) ;
#7303 = ORIENTED_EDGE ( 'NONE', *, *, #7218, .F. ) ;
#7304 = FACE_OUTER_BOUND ( 'NONE', #4690, .T. ) ;
#7305 = ORIENTED_EDGE ( 'NONE', *, *, #400, .F. ) ;
#7306 = ORIENTED_EDGE ( 'NONE', *, *, #8141, .F. ) ;
#7307 = DIRECTION ( 'NONE',  ( -2.168404344971008621E-16, 1.000000000000000000, 0.000000000000000000 ) ) ;
#7308 = EDGE_CURVE ( 'NONE', #480, #6188, #2565, .T. ) ;
#7309 = CARTESIAN_POINT ( 'NONE',  ( 60.00000000000004263, 85.00000000000051159, 2.399999999999971489 ) ) ;
#7310 = DIRECTION ( 'NONE',  ( -0.000000000000000000, -0.000000000000000000, 1.000000000000000000 ) ) ;
#7311 = CARTESIAN_POINT ( 'NONE',  ( -6.954674599839328231, 0.9195257330843505938, 8.033525432897004492 ) ) ;
#7312 = DIRECTION ( 'NONE',  ( 0.000000000000000000, 0.5000000000000009992, 0.8660254037844380415 ) ) ;
#7313 = APPLICATION_PROTOCOL_DEFINITION ( 'draft international standard', 'automotive_design', 1998, #2541 ) ;
#7314 = ORIENTED_EDGE ( 'NONE', *, *, #6031, .T. ) ;
#7315 = ORIENTED_EDGE ( 'NONE', *, *, #1028, .F. ) ;
#7316 = ORIENTED_EDGE ( 'NONE', *, *, #4937, .F. ) ;
#7317 = CARTESIAN_POINT ( 'NONE',  ( 0.000000000000000000, -2.357898499370430834, 3.469446951953614189E-15 ) ) ;
#7318 = CARTESIAN_POINT ( 'NONE',  ( 4.622735087487665595, -5.276717374392886128, 8.014740495741826010 ) ) ;
#7319 = DIRECTION ( 'NONE',  ( 1.412205397084881070E-17, -2.775557561562891967E-17, -1.000000000000000000 ) ) ;
#7320 = CONICAL_SURFACE ( 'NONE', #2567, 1.250000000000001110, 1.029744258676655200 ) ;
#7321 = ORIENTED_EDGE ( 'NONE', *, *, #2492, .F. ) ;
#7322 = CARTESIAN_POINT ( 'NONE',  ( 4.000000000000000000, 0.000000000000000000, 0.000000000000000000 ) ) ;
#7323 = EDGE_CURVE ( 'NONE', #166, #6955, #5676, .T. ) ;
#7324 = AXIS2_PLACEMENT_3D ( 'NONE', #5309, #7829, #299 ) ;
#7325 = PLANE ( 'NONE',  #3041 ) ;
#7326 = DIRECTION ( 'NONE',  ( 0.000000000000000000, 0.000000000000000000, -1.000000000000000000 ) ) ;
#7327 = CARTESIAN_POINT ( 'NONE',  ( -6.554102889824980238, -2.469088713791839140, 8.029774298059875193 ) ) ;
#7328 = DIRECTION ( 'NONE',  ( -0.000000000000000000, -0.000000000000000000, 1.000000000000000000 ) ) ;
#7329 = EDGE_CURVE ( 'NONE', #2818, #7111, #3716, .T. ) ;
#7330 = VERTEX_POINT ( 'NONE', #7742 ) ;
#7331 = ORIENTED_EDGE ( 'NONE', *, *, #4735, .F. ) ;
#7332 = FACE_OUTER_BOUND ( 'NONE', #7811, .T. ) ;
#7333 = CARTESIAN_POINT ( 'NONE',  ( 2.000000000000000000, -0.8865213383406721492, -1.535499999999998977 ) ) ;
#7334 = DIRECTION ( 'NONE',  ( 0.000000000000000000, 0.000000000000000000, -1.000000000000000000 ) ) ;
#7335 = CARTESIAN_POINT ( 'NONE',  ( 1.300000000000000044, 0.7390083445627224634, 1.279999999999999138 ) ) ;
#7336 = DIRECTION ( 'NONE',  ( 0.000000000000000000, 0.000000000000000000, -1.000000000000000000 ) ) ;
#7337 = PLANE ( 'NONE',  #2419 ) ;
#7338 = EDGE_LOOP ( 'NONE', ( #5171, #6238, #7473 ) ) ;
#7339 = FACE_OUTER_BOUND ( 'NONE', #4257, .T. ) ;
#7340 = ORIENTED_EDGE ( 'NONE', *, *, #6483, .T. ) ;
#7341 = EDGE_CURVE ( 'NONE', #2250, #5593, #6757, .T. ) ;
#7342 = ORIENTED_EDGE ( 'NONE', *, *, #1009, .F. ) ;
#7343 = PRESENTATION_LAYER_ASSIGNMENT (  '', '', ( #5634 ) ) ;
#7344 = ADVANCED_FACE ( 'NONE', ( #5065, #1475 ), #7814, .T. ) ;
#7345 = CARTESIAN_POINT ( 'NONE',  ( 4.999999999999990230, 0.000000000000000000, 20.00000000000000355 ) ) ;
#7346 = EDGE_CURVE ( 'NONE', #4997, #4218, #611, .T. ) ;
#7347 = DIRECTION ( 'NONE',  ( -1.734723475976806848E-16, 1.000000000000000000, -0.000000000000000000 ) ) ;
#7348 = DIRECTION ( 'NONE',  ( 1.000000000000000000, 0.000000000000000000, 0.000000000000000000 ) ) ;
#7349 = CARTESIAN_POINT ( 'NONE',  ( -6.377569469000553326, 2.894565604611681664, 8.028191719259677228 ) ) ;
#7350 = CARTESIAN_POINT ( 'NONE',  ( 57.99999999999999289, 7.999999999999996447, 11.99999999999998934 ) ) ;
#7351 = ITEM_DEFINED_TRANSFORMATION ( 'NONE', 'NONE', #1513,  #1587 ) ;
#7352 = ORIENTED_EDGE ( 'NONE', *, *, #6571, .T. ) ;
#7353 = ORIENTED_EDGE ( 'NONE', *, *, #4168, .T. ) ;
#7354 = ORIENTED_EDGE ( 'NONE', *, *, #5976, .F. ) ;
#7355 = FACE_OUTER_BOUND ( 'NONE', #704, .T. ) ;
#7356 = DIRECTION ( 'NONE',  ( -1.000000000000000000, 0.000000000000000000, 0.000000000000000000 ) ) ;
#7357 = CARTESIAN_POINT ( 'NONE',  ( 1.270137496355039850E-14, 85.00000000000011369, 5.000000000000046185 ) ) ;
#7358 = ORIENTED_EDGE ( 'NONE', *, *, #1387, .T. ) ;
#7359 = DIRECTION ( 'NONE',  ( -0.000000000000000000, 1.000000000000000000, -0.000000000000000000 ) ) ;
#7360 = ORIENTED_EDGE ( 'NONE', *, *, #7946, .F. ) ;
#7361 = LINE ( 'NONE', #6160, #5713 ) ;
#7362 = DIRECTION ( 'NONE',  ( 0.000000000000000000, 1.000000000000000000, -1.100686371591861952E-15 ) ) ;
#7363 =( LENGTH_UNIT ( ) NAMED_UNIT ( * ) SI_UNIT ( .MILLI., .METRE. ) );
#7364 = SURFACE_STYLE_FILL_AREA ( #560 ) ;
#7365 = UNCERTAINTY_MEASURE_WITH_UNIT (LENGTH_MEASURE( 1.000000000000000082E-05 ), #5891, 'distance_accuracy_value', 'NONE');
#7366 = CARTESIAN_POINT ( 'NONE',  ( 1.300000000000000044, 1.478016689125442484, -1.626303258728256651E-15 ) ) ;
#7367 = EDGE_CURVE ( 'NONE', #7189, #531, #7952, .T. ) ;
#7368 = ORIENTED_EDGE ( 'NONE', *, *, #167, .T. ) ;
#7369 = ORIENTED_EDGE ( 'NONE', *, *, #5611, .F. ) ;
#7370 = DIRECTION ( 'NONE',  ( 0.000000000000000000, 0.000000000000000000, 1.000000000000000000 ) ) ;
#7371 = CARTESIAN_POINT ( 'NONE',  ( -2.000000000000022649, -3.464101615137742396, -2.700000000000001066 ) ) ;
#7372 = CARTESIAN_POINT ( 'NONE',  ( 60.00000000000014211, 10.00000000000000000, 10.50000000000006395 ) ) ;
#7373 = CARTESIAN_POINT ( 'NONE',  ( 0.000000000000000000, 0.000000000000000000, 0.000000000000000000 ) ) ;
#7374 = DIRECTION ( 'NONE',  ( 0.000000000000000000, 0.000000000000000000, 1.000000000000000000 ) ) ;
#7375 = DIRECTION ( 'NONE',  ( 0.000000000000000000, 0.000000000000000000, 1.000000000000000000 ) ) ;
#7376 = ORIENTED_EDGE ( 'NONE', *, *, #556, .F. ) ;
#7377 = AXIS2_PLACEMENT_3D ( 'NONE', #1337, #5888, #35 ) ;
#7378 = DIRECTION ( 'NONE',  ( 1.000000000000000000, 0.000000000000000000, 0.000000000000000000 ) ) ;
#7379 = VECTOR ( 'NONE', #5030, 1000.000000000000000 ) ;
#7380 = ADVANCED_FACE ( 'NONE', ( #2835 ), #326, .F. ) ;
#7381 = ORIENTED_EDGE ( 'NONE', *, *, #1274, .T. ) ;
#7382 = VERTEX_POINT ( 'NONE', #2871 ) ;
#7383 = CARTESIAN_POINT ( 'NONE',  ( 2.000000000000010658, -3.464101615137748169, 0.000000000000000000 ) ) ;
#7384 = LINE ( 'NONE', #6103, #2369 ) ;
#7385 = LINE ( 'NONE', #1703, #3758 ) ;
#7386 = CARTESIAN_POINT ( 'NONE',  ( 1.300000000000000044, -1.478016689125442706, 1.843143693225357538E-15 ) ) ;
#7387 = CARTESIAN_POINT ( 'NONE',  ( 2.000000000000000000, -1.329782007511006281, -0.7677499999999984892 ) ) ;
#7388 = ITEM_DEFINED_TRANSFORMATION ( 'NONE', 'NONE', #3638,  #1587 ) ;
#7389 = EDGE_CURVE ( 'NONE', #7060, #7949, #1595, .T. ) ;
#7390 = CIRCLE ( 'NONE', #5415, 2.149999999999995470 ) ;
#7391 = ORIENTED_EDGE ( 'NONE', *, *, #2608, .T. ) ;
#7392 = AXIS2_PLACEMENT_3D ( 'NONE', #648, #758, #5804 ) ;
#7393 = EDGE_LOOP ( 'NONE', ( #1532, #260, #2676, #6289, #5831 ) ) ;
#7394 = ORIENTED_EDGE ( 'NONE', *, *, #2986, .T. ) ;
#7395 = DIRECTION ( 'NONE',  ( 0.000000000000000000, 0.000000000000000000, 1.000000000000000000 ) ) ;
#7396 = DIRECTION ( 'NONE',  ( -0.000000000000000000, -0.000000000000000000, 1.000000000000000000 ) ) ;
#7397 = CARTESIAN_POINT ( 'NONE',  ( 3.000000000000000888, 35.09008114612887397, 0.000000000000000000 ) ) ;
#7398 = VECTOR ( 'NONE', #848, 1000.000000000000000 ) ;
#7399 = CIRCLE ( 'NONE', #4225, 0.2000000000000000944 ) ;
#7400 = ORIENTED_EDGE ( 'NONE', *, *, #1521, .T. ) ;
#7401 = CARTESIAN_POINT ( 'NONE',  ( 0.000000000000000000, 0.000000000000000000, 10.00000000000000000 ) ) ;
#7402 = EDGE_LOOP ( 'NONE', ( #3533, #1811 ) ) ;
#7403 = EDGE_LOOP ( 'NONE', ( #3253, #1640, #7979, #2193 ) ) ;
#7404 = CIRCLE ( 'NONE', #2110, 4.999999999999993783 ) ;
#7405 = AXIS2_PLACEMENT_3D ( 'NONE', #7223, #6590, #4614 ) ;
#7406 = FACE_BOUND ( 'NONE', #2456, .T. ) ;
#7407 = ADVANCED_FACE ( 'NONE', ( #4125 ), #6603, .F. ) ;
#7408 = CARTESIAN_POINT ( 'NONE',  ( 0.000000000000000000, 0.000000000000000000, 0.000000000000000000 ) ) ;
#7409 = ADVANCED_FACE ( 'NONE', ( #2132 ), #7154, .F. ) ;
#7410 = EDGE_CURVE ( 'NONE', #6416, #6473, #6098, .T. ) ;
#7411 = DIRECTION ( 'NONE',  ( 1.000000000000000000, 0.000000000000000000, 0.000000000000000000 ) ) ;
#7412 = AXIS2_PLACEMENT_3D ( 'NONE', #2284, #6055, #357 ) ;
#7413 = CARTESIAN_POINT ( 'NONE',  ( 0.000000000000000000, 0.000000000000000000, 20.00000000000000355 ) ) ;
#7414 = VECTOR ( 'NONE', #5614, 1000.000000000000000 ) ;
#7415 = CONICAL_SURFACE ( 'NONE', #6110, 4.000000000000000000, 1.047197551196595855 ) ;
#7416 = EDGE_LOOP ( 'NONE', ( #5133, #3371 ) ) ;
#7417 = ORIENTED_EDGE ( 'NONE', *, *, #5661, .F. ) ;
#7418 = AXIS2_PLACEMENT_3D ( 'NONE', #5649, #6135, #4350 ) ;
#7419 = AXIS2_PLACEMENT_3D ( 'NONE', #7153, #285, #202 ) ;
#7420 = DIRECTION ( 'NONE',  ( 0.000000000000000000, 1.000000000000000000, 0.000000000000000000 ) ) ;
#7421 = DIRECTION ( 'NONE',  ( 1.412205397084881070E-17, -2.775557561562891967E-17, -1.000000000000000000 ) ) ;
#7422 = LINE ( 'NONE', #6837, #2533 ) ;
#7423 = VECTOR ( 'NONE', #6124, 1000.000000000000000 ) ;
#7424 = LINE ( 'NONE', #4272, #124 ) ;
#7425 = DIRECTION ( 'NONE',  ( -1.000000000000000000, 0.000000000000000000, -0.000000000000000000 ) ) ;
#7426 = PRODUCT_DEFINITION_SHAPE ( 'NONE', 'NONE',  #5748 ) ;
#7427 = ORIENTED_EDGE ( 'NONE', *, *, #6775, .T. ) ;
#7428 = AXIS2_PLACEMENT_3D ( 'NONE', #3922, #6410, #1260 ) ;
#7429 = ORIENTED_EDGE ( 'NONE', *, *, #6480, .T. ) ;
#7430 = DIRECTION ( 'NONE',  ( 0.000000000000000000, 0.000000000000000000, -1.000000000000000000 ) ) ;
#7431 = CARTESIAN_POINT ( 'NONE',  ( 24.00000000000000000, 0.000000000000000000, 1.610000000000000098 ) ) ;
#7432 = CARTESIAN_POINT ( 'NONE',  ( 2.000000000000000000, -0.8865213383406685965, 1.535500000000000531 ) ) ;
#7433 = DIRECTION ( 'NONE',  ( 0.000000000000000000, -0.8660254037844390407, -0.4999999999999993339 ) ) ;
#7434 = EDGE_CURVE ( 'NONE', #4369, #5370, #875, .T. ) ;
#7435 = CARTESIAN_POINT ( 'NONE',  ( 2.500000000000002220, 0.000000000000000000, -25.03750572909317285 ) ) ;
#7436 = DIRECTION ( 'NONE',  ( -0.000000000000000000, 1.320393690296331133E-15, 1.000000000000000000 ) ) ;
#7437 = PRESENTATION_LAYER_ASSIGNMENT (  '', '', ( #2792 ) ) ;
#7438 = ITEM_DEFINED_TRANSFORMATION ( 'NONE', 'NONE', #305,  #1587 ) ;
#7439 = ORIENTED_EDGE ( 'NONE', *, *, #1750, .T. ) ;
#7440 = PRESENTATION_LAYER_ASSIGNMENT (  '', '', ( #2134 ) ) ;
#7441 = VERTEX_POINT ( 'NONE', #1637 ) ;
#7442 = ORIENTED_EDGE ( 'NONE', *, *, #6591, .T. ) ;
#7443 = EDGE_LOOP ( 'NONE', ( #3225, #13, #4135, #633 ) ) ;
#7444 = FACE_OUTER_BOUND ( 'NONE', #1711, .T. ) ;
#7445 = DIRECTION ( 'NONE',  ( 1.000000000000000000, 0.000000000000000000, 0.000000000000000000 ) ) ;
#7446 = CARTESIAN_POINT ( 'NONE',  ( 9.020562075079396891E-14, -10.00000000000000000, 729.2499999999977263 ) ) ;
#7447 = UNCERTAINTY_MEASURE_WITH_UNIT (LENGTH_MEASURE( 1.000000000000000082E-05 ), #6567, 'distance_accuracy_value', 'NONE');
#7448 = SHAPE_REPRESENTATION_RELATIONSHIP ( 'NONE' , 'NONE' ,  #7870, #7647 ) ;
#7449 = VERTEX_POINT ( 'NONE', #4164 ) ;
#7450 = CARTESIAN_POINT ( 'NONE',  ( 1.270137496355039850E-14, 85.00000000000011369, 5.000000000000046185 ) ) ;
#7451 = ORIENTED_EDGE ( 'NONE', *, *, #6099, .T. ) ;
#7452 = EDGE_LOOP ( 'NONE', ( #1023, #1385 ) ) ;
#7453 = EDGE_CURVE ( 'NONE', #7616, #4584, #1601, .T. ) ;
#7454 = CARTESIAN_POINT ( 'NONE',  ( 9.020562075079396891E-14, -10.00000000000000000, 729.2499999999977263 ) ) ;
#7455 = EDGE_CURVE ( 'NONE', #931, #3615, #5872, .T. ) ;
#7456 = DIRECTION ( 'NONE',  ( 1.000000000000000000, 0.000000000000000000, 0.000000000000000000 ) ) ;
#7457 = CARTESIAN_POINT ( 'NONE',  ( 0.9164596775857979383, 6.954740550032190605, 8.000443323644105931 ) ) ;
#7458 = B_SPLINE_CURVE_WITH_KNOTS ( 'NONE', 3,
 ( #1564, #1652, #1063, #432, #6133, #3558 ),
 .UNSPECIFIED., .F., .F.,
 ( 4, 2, 4 ),
 ( 0.002336974151641604998, 0.003500975885716476645, 0.004664977619791348291 ),
 .UNSPECIFIED. ) ;
#7459 = PRODUCT_RELATED_PRODUCT_CATEGORY ( 'part', '', ( #1876 ) ) ;
#7460 = CIRCLE ( 'NONE', #3090, 1.535500000000000087 ) ;
#7461 = ORIENTED_EDGE ( 'NONE', *, *, #1058, .F. ) ;
#7462 = ORIENTED_EDGE ( 'NONE', *, *, #2444, .T. ) ;
#7463 = FILL_AREA_STYLE ('',( #4268 ) ) ;
#7464 = CARTESIAN_POINT ( 'NONE',  ( -30.00000000000000355, -29.99999999999999289, 1.734723475976807094E-15 ) ) ;
#7465 = CARTESIAN_POINT ( 'NONE',  ( 40.00000000000000711, 40.00000000000000711, 10.00000000000000000 ) ) ;
#7466 = DIRECTION ( 'NONE',  ( 0.000000000000000000, 0.000000000000000000, 1.000000000000000000 ) ) ;
#7467 = FACE_OUTER_BOUND ( 'NONE', #3849, .T. ) ;
#7468 = AXIS2_PLACEMENT_3D ( 'NONE', #3695, #5615, #3076 ) ;
#7469 = LINE ( 'NONE', #4229, #3535 ) ;
#7470 = EDGE_CURVE ( 'NONE', #4267, #6924, #5463, .T. ) ;
#7471 = VERTEX_POINT ( 'NONE', #369 ) ;
#7472 = ADVANCED_FACE ( 'NONE', ( #4871 ), #8054, .F. ) ;
#7473 = ORIENTED_EDGE ( 'NONE', *, *, #386, .F. ) ;
#7474 = CARTESIAN_POINT ( 'NONE',  ( -7.000000000000000000, 0.000000000000000000, 10.00000000000000000 ) ) ;
#7475 = CARTESIAN_POINT ( 'NONE',  ( 1.300000000000000044, 0.000000000000000000, 0.000000000000000000 ) ) ;
#7476 = LINE ( 'NONE', #7432, #7274 ) ;
#7477 = DIRECTION ( 'NONE',  ( -1.000000000000000000, 0.000000000000000000, 0.000000000000000000 ) ) ;
#7478 = STYLED_ITEM ( 'NONE', ( #1434 ), #6151 ) ;
#7479 = LINE ( 'NONE', #6398, #4746 ) ;
#7480 = PLANE ( 'NONE',  #7540 ) ;
#7481 = ITEM_DEFINED_TRANSFORMATION ( 'NONE', 'NONE', #7210,  #1587 ) ;
#7482 = ORIENTED_EDGE ( 'NONE', *, *, #3106, .F. ) ;
#7483 = EDGE_CURVE ( 'NONE', #6246, #6819, #3626, .T. ) ;
#7484 = ORIENTED_EDGE ( 'NONE', *, *, #1983, .T. ) ;
#7485 = VERTEX_POINT ( 'NONE', #2991 ) ;
#7486 = VERTEX_POINT ( 'NONE', #6066 ) ;
#7487 = CARTESIAN_POINT ( 'NONE',  ( 2.000000000000000000, 0.8865213383406687075, -1.535500000000000975 ) ) ;
#7488 = DIRECTION ( 'NONE',  ( 0.000000000000000000, 0.000000000000000000, 1.000000000000000000 ) ) ;
#7489 = CARTESIAN_POINT ( 'NONE',  ( 0.000000000000000000, 0.000000000000000000, -2.700000000000000178 ) ) ;
#7490 = STYLED_ITEM ( 'NONE', ( #498 ), #7647 ) ;
#7491 = ORIENTED_EDGE ( 'NONE', *, *, #4864, .F. ) ;
#7492 = FACE_OUTER_BOUND ( 'NONE', #170, .T. ) ;
#7493 = ORIENTED_EDGE ( 'NONE', *, *, #6820, .T. ) ;
#7494 = VECTOR ( 'NONE', #3208, 1000.000000000000114 ) ;
#7495 = ORIENTED_EDGE ( 'NONE', *, *, #5351, .F. ) ;
#7496 = PLANE ( 'NONE',  #6481 ) ;
#7497 = DIRECTION ( 'NONE',  ( -1.000000000000000000, 0.000000000000000000, 0.000000000000000000 ) ) ;
#7498 = SURFACE_STYLE_FILL_AREA ( #8193 ) ;
#7499 = PRODUCT ( 'socket head cap screw_iso_ISO 4762 M4 x 16 - 16N', 'socket head cap screw_iso_ISO 4762 M4 x 16 - 16N', '', ( #906 ) ) ;
#7500 = CARTESIAN_POINT ( 'NONE',  ( 0.1999999999999987899, 4.286263797015736595E-16, -3.500000000000000000 ) ) ;
#7501 = ORIENTED_EDGE ( 'NONE', *, *, #5785, .F. ) ;
#7502 = ORIENTED_EDGE ( 'NONE', *, *, #4034, .F. ) ;
#7503 = SURFACE_SIDE_STYLE ('',( #4346 ) ) ;
#7504 = CARTESIAN_POINT ( 'NONE',  ( -31.74999999999994316, 3.061616997868383634E-16, -2.500000000000000444 ) ) ;
#7505 = DIRECTION ( 'NONE',  ( -0.000000000000000000, -0.000000000000000000, 1.000000000000000000 ) ) ;
#7506 = DIRECTION ( 'NONE',  ( 0.000000000000000000, 0.000000000000000000, -1.000000000000000000 ) ) ;
#7507 = CARTESIAN_POINT ( 'NONE',  ( 1.300000000000000044, 1.478016689125442484, -1.626303258728256651E-15 ) ) ;
#7508 = FACE_OUTER_BOUND ( 'NONE', #4036, .T. ) ;
#7509 = ORIENTED_EDGE ( 'NONE', *, *, #1647, .F. ) ;
#7510 = LINE ( 'NONE', #5613, #1182 ) ;
#7511 = CARTESIAN_POINT ( 'NONE',  ( 2.000000000000000000, 0.000000000000000000, 0.000000000000000000 ) ) ;
#7512 = DIRECTION ( 'NONE',  ( 0.000000000000000000, 1.000000000000000000, -0.000000000000000000 ) ) ;
#7513 = CARTESIAN_POINT ( 'NONE',  ( -1.599999999999998979, 37.49999999999999289, 0.000000000000000000 ) ) ;
#7514 = CARTESIAN_POINT ( 'NONE',  ( 1.084202172485504434E-14, 4.618802153517020948, -2.342734410091827701 ) ) ;
#7515 = EDGE_CURVE ( 'NONE', #3165, #3286, #3734, .T. ) ;
#7516 = EDGE_CURVE ( 'NONE', #5129, #6340, #4963, .T. ) ;
#7517 = CARTESIAN_POINT ( 'NONE',  ( 2.000000000000010658, -3.464101615137748169, 0.000000000000000000 ) ) ;
#7518 = AXIS2_PLACEMENT_3D ( 'NONE', #8060, #5504, #462 ) ;
#7519 = CONTEXT_DEPENDENT_SHAPE_REPRESENTATION ( #2627, #5727 ) ;
#7520 = ADVANCED_FACE ( 'NONE', ( #7975 ), #5498, .F. ) ;
#7521 = ORIENTED_EDGE ( 'NONE', *, *, #7847, .T. ) ;
#7522 = ORIENTED_EDGE ( 'NONE', *, *, #4285, .F. ) ;
#7523 = ORIENTED_EDGE ( 'NONE', *, *, #7565, .T. ) ;
#7524 = ORIENTED_EDGE ( 'NONE', *, *, #3771, .T. ) ;
#7525 = CARTESIAN_POINT ( 'NONE',  ( -41.97904239022134476, 83.67335008385822448, 2.000000000000043521 ) ) ;
#7526 = CARTESIAN_POINT ( 'NONE',  ( 2.649999999999991918, 0.000000000000000000, 1.040834085586084257E-14 ) ) ;
#7527 = DIRECTION ( 'NONE',  ( 0.000000000000000000, -0.000000000000000000, 1.000000000000000000 ) ) ;
#7528 = CARTESIAN_POINT ( 'NONE',  ( 0.000000000000000000, 16.01196202519846068, 0.000000000000000000 ) ) ;
#7529 = ORIENTED_EDGE ( 'NONE', *, *, #3650, .F. ) ;
#7530 = DIRECTION ( 'NONE',  ( -1.000000000000000000, -0.000000000000000000, -0.000000000000000000 ) ) ;
#7531 = ORIENTED_EDGE ( 'NONE', *, *, #7367, .F. ) ;
#7532 = VERTEX_POINT ( 'NONE', #7526 ) ;
#7533 = CIRCLE ( 'NONE', #5026, 2.649999999999999467 ) ;
#7534 = CARTESIAN_POINT ( 'NONE',  ( 5.000000000000015099, 5.204748896376250699E-16, -4.250000000000000000 ) ) ;
#7535 = PLANE ( 'NONE',  #2524 ) ;
#7536 = LINE ( 'NONE', #4468, #1304 ) ;
#7537 = MECHANICAL_DESIGN_GEOMETRIC_PRESENTATION_REPRESENTATION (  '', ( #1437 ), #1976 ) ;
#7538 = ADVANCED_FACE ( 'NONE', ( #2463 ), #4251, .T. ) ;
#7539 = FACE_OUTER_BOUND ( 'NONE', #544, .T. ) ;
#7540 = AXIS2_PLACEMENT_3D ( 'NONE', #7609, #3660, #4323 ) ;
#7541 = CARTESIAN_POINT ( 'NONE',  ( -1.198153218366585720E-14, 42.68016229225776925, 4.000000000000001776 ) ) ;
#7542 = AXIS2_PLACEMENT_3D ( 'NONE', #3281, #7297, #5354 ) ;
#7543 = ADVANCED_FACE ( 'NONE', ( #8015 ), #5313, .T. ) ;
#7544 = AXIS2_PLACEMENT_3D ( 'NONE', #5135, #78, #5097 ) ;
#7545 = VERTEX_POINT ( 'NONE', #1763 ) ;
#7546 = ORIENTED_EDGE ( 'NONE', *, *, #4393, .T. ) ;
#7547 = DIRECTION ( 'NONE',  ( -0.000000000000000000, -0.000000000000000000, 1.000000000000000000 ) ) ;
#7548 = CARTESIAN_POINT ( 'NONE',  ( 60.00000000000000711, 9.332579536216795825E-15, 53.34999999999998721 ) ) ;
#7549 = FACE_OUTER_BOUND ( 'NONE', #1130, .T. ) ;
#7550 = VECTOR ( 'NONE', #7697, 1000.000000000000000 ) ;
#7551 = CARTESIAN_POINT ( 'NONE',  ( -58.00000000000006395, 7.999999999999996447, 11.99999999999998934 ) ) ;
#7552 = VECTOR ( 'NONE', #3830, 1000.000000000000114 ) ;
#7553 = AXIS2_PLACEMENT_3D ( 'NONE', #2530, #3199, #3740 ) ;
#7554 = DIRECTION ( 'NONE',  ( -0.000000000000000000, -0.000000000000000000, 1.000000000000000000 ) ) ;
#7555 = PLANE ( 'NONE',  #4867 ) ;
#7556 = ORIENTED_EDGE ( 'NONE', *, *, #3057, .T. ) ;
#7557 = CIRCLE ( 'NONE', #521, 1.500000000000000222 ) ;
#7558 = DIRECTION ( 'NONE',  ( 1.000000000000000000, 0.000000000000000000, 0.000000000000000000 ) ) ;
#7559 = EDGE_CURVE ( 'NONE', #2397, #2418, #8091, .T. ) ;
#7561 = CARTESIAN_POINT ( 'NONE',  ( 60.00000000000004263, 85.00000000000051159, -2.399999999999999467 ) ) ;
#7560 = AXIS2_PLACEMENT_3D ( 'NONE', #7199, #5471, #1515 ) ;
#7562 = FACE_OUTER_BOUND ( 'NONE', #451, .T. ) ;
#7563 = DIRECTION ( 'NONE',  ( 0.000000000000000000, 0.000000000000000000, 1.000000000000000000 ) ) ;
#7564 = CARTESIAN_POINT ( 'NONE',  ( -4.000000000000000000, 2.309401076758496263, -0.3572655899081631503 ) ) ;
#7565 = EDGE_CURVE ( 'NONE', #3093, #2445, #3668, .T. ) ;
#7566 = CARTESIAN_POINT ( 'NONE',  ( 49.99683717277851258, 85.63216245974612661, -2.336254100262029176 ) ) ;
#7567 = EDGE_LOOP ( 'NONE', ( #4010, #387 ) ) ;
#7568 = AXIS2_PLACEMENT_3D ( 'NONE', #866, #1508, #7272 ) ;
#7569 = AXIS2_PLACEMENT_3D ( 'NONE', #3825, #2350, #8162 ) ;
#7570 = ORIENTED_EDGE ( 'NONE', *, *, #2756, .F. ) ;
#7571 = PRODUCT_DEFINITION ( 'UNKNOWN', '', #1099, #4651 ) ;
#7572 = CARTESIAN_POINT ( 'NONE',  ( 2.000000000000000000, 1.773042676681340968, -2.276824562219559311E-15 ) ) ;
#7573 = PRODUCT_DEFINITION_CONTEXT ( 'detailed design', #3646, 'design' ) ;
#7574 = VERTEX_POINT ( 'NONE', #4920 ) ;
#7575 = ORIENTED_EDGE ( 'NONE', *, *, #505, .F. ) ;
#7576 = AXIS2_PLACEMENT_3D ( 'NONE', #5015, #3898, #6421 ) ;
#7577 = LINE ( 'NONE', #1843, #1709 ) ;
#7578 = LINE ( 'NONE', #7, #4921 ) ;
#7579 = AXIS2_PLACEMENT_3D ( 'NONE', #5115, #4021, #759 ) ;
#7580 = CARTESIAN_POINT ( 'NONE',  ( 55.00000000000000000, -8.000000000000001776, -2.849999999999991651 ) ) ;
#7581 = CARTESIAN_POINT ( 'NONE',  ( -55.00000000000000000, 41.51196202519846423, 14.00000000000000000 ) ) ;
#7582 = AXIS2_PLACEMENT_3D ( 'NONE', #4022, #4750, #7125 ) ;
#7583 = ORIENTED_EDGE ( 'NONE', *, *, #6301, .T. ) ;
#7584 = LINE ( 'NONE', #190, #6706 ) ;
#7585 = ORIENTED_EDGE ( 'NONE', *, *, #4960, .F. ) ;
#7586 = ORIENTED_EDGE ( 'NONE', *, *, #7207, .F. ) ;
#7587 =( REPRESENTATION_RELATIONSHIP ('NONE','NONE', #3916, #6987 ) REPRESENTATION_RELATIONSHIP_WITH_TRANSFORMATION ( #7351 )SHAPE_REPRESENTATION_RELATIONSHIP( ) );
#7588 = ADVANCED_FACE ( 'NONE', ( #547 ), #2296, .F. ) ;
#7589 = FACE_BOUND ( 'NONE', #1252, .T. ) ;
#7590 = CARTESIAN_POINT ( 'NONE',  ( 2.000000000000000000, 0.000000000000000000, 0.000000000000000000 ) ) ;
#7591 = FACE_OUTER_BOUND ( 'NONE', #5297, .T. ) ;
#7592 = DIRECTION ( 'NONE',  ( -0.000000000000000000, -0.000000000000000000, 1.000000000000000000 ) ) ;
#7593 = ADVANCED_FACE ( 'NONE', ( #2331 ), #1878, .F. ) ;
#7594 = DIRECTION ( 'NONE',  ( -0.000000000000000000, 0.8660254037844391517, 0.4999999999999991118 ) ) ;
#7595 = ORIENTED_EDGE ( 'NONE', *, *, #2137, .T. ) ;
#7596 = ORIENTED_EDGE ( 'NONE', *, *, #5275, .T. ) ;
#7597 = SURFACE_STYLE_FILL_AREA ( #431 ) ;
#7598 = DIRECTION ( 'NONE',  ( -0.000000000000000000, -0.000000000000000000, 1.000000000000000000 ) ) ;
#7599 = DIRECTION ( 'NONE',  ( 0.000000000000000000, 0.000000000000000000, -1.000000000000000000 ) ) ;
#7600 = CARTESIAN_POINT ( 'NONE',  ( 0.000000000000000000, 37.49999999999999289, 4.000000000000001776 ) ) ;
#7601 = DIRECTION ( 'NONE',  ( 0.000000000000000000, 0.000000000000000000, 1.000000000000000000 ) ) ;
#7602 = CARTESIAN_POINT ( 'NONE',  ( -49.94811673897444848, 87.27799541866311017, 0.7717081223120660916 ) ) ;
#7603 = AXIS2_PLACEMENT_3D ( 'NONE', #1663, #407, #2947 ) ;
#7604 = VERTEX_POINT ( 'NONE', #6815 ) ;
#7605 = CARTESIAN_POINT ( 'NONE',  ( 24.99999999999998224, 30.00000000000001421, 10.00000000000000000 ) ) ;
#7606 = DIRECTION ( 'NONE',  ( 1.000000000000000000, 0.000000000000000000, 0.000000000000000000 ) ) ;
#7607 = CARTESIAN_POINT ( 'NONE',  ( 0.000000000000000000, 0.000000000000000000, 0.000000000000000000 ) ) ;
#7608 = CARTESIAN_POINT ( 'NONE',  ( -1.660531772554312280, 3.660093687634850212, -2.700000000000004174 ) ) ;
#7609 = CARTESIAN_POINT ( 'NONE',  ( 2.000000000000000000, 1.773042676681340968, -2.276824562219559311E-15 ) ) ;
#7610 = VERTEX_POINT ( 'NONE', #6192 ) ;
#7611 = ADVANCED_FACE ( 'NONE', ( #5587 ), #5849, .F. ) ;
#7612 = ORIENTED_EDGE ( 'NONE', *, *, #7848, .F. ) ;
#7613 = EDGE_CURVE ( 'NONE', #1975, #2468, #6380, .T. ) ;
#7614 = FACE_OUTER_BOUND ( 'NONE', #3218, .T. ) ;
#7615 = ORIENTED_EDGE ( 'NONE', *, *, #5149, .T. ) ;
#7616 = VERTEX_POINT ( 'NONE', #126 ) ;
#7617 = CARTESIAN_POINT ( 'NONE',  ( 11.00000000000000355, 1.665213485140613626E-16, -1.219500000000000028 ) ) ;
#7618 = DIRECTION ( 'NONE',  ( 0.000000000000000000, 0.000000000000000000, -1.000000000000000000 ) ) ;
#7619 = DIRECTION ( 'NONE',  ( 0.000000000000000000, 0.000000000000000000, 1.000000000000000000 ) ) ;
#7620 = ORIENTED_EDGE ( 'NONE', *, *, #7826, .F. ) ;
#7621 = ORIENTED_EDGE ( 'NONE', *, *, #2929, .F. ) ;
#7622 = VERTEX_POINT ( 'NONE', #3761 ) ;
#7623 = AXIS2_PLACEMENT_3D ( 'NONE', #713, #3803, #6412 ) ;
#7624 = CARTESIAN_POINT ( 'NONE',  ( 1.250000000000004441, 38.99999999999999289, -4.999999999999990230 ) ) ;
#7625 = CARTESIAN_POINT ( 'NONE',  ( 41.94739886896327619, 87.10210726516650936, -1.165086683815467206 ) ) ;
#7626 = DIRECTION ( 'NONE',  ( -0.000000000000000000, -0.000000000000000000, 1.000000000000000000 ) ) ;
#7627 = SURFACE_STYLE_USAGE ( .BOTH. , #91 ) ;
#7628 = FILL_AREA_STYLE_COLOUR ( '', #2537 ) ;
#7629 = VECTOR ( 'NONE', #4056, 1000.000000000000000 ) ;
#7630 = APPLICATION_CONTEXT ( 'automotive_design' ) ;
#7631 = VERTEX_POINT ( 'NONE', #1389 ) ;
#7632 = LINE ( 'NONE', #4477, #5843 ) ;
#7633 = FACE_BOUND ( 'NONE', #4256, .T. ) ;
#7634 = DIRECTION ( 'NONE',  ( 1.000000000000000000, 0.000000000000000000, -2.065146995210483462E-17 ) ) ;
#7635 = PLANE ( 'NONE',  #5569 ) ;
#7636 = ADVANCED_FACE ( 'NONE', ( #3131 ), #5173, .T. ) ;
#7637 = CYLINDRICAL_SURFACE ( 'NONE', #6636, 2.149999999999995470 ) ;
#7638 = CARTESIAN_POINT ( 'NONE',  ( 4.999999999999993783, 6.123233995736758394E-16, 5.400000000000002132 ) ) ;
#7639 = EDGE_LOOP ( 'NONE', ( #3262, #6320, #984, #7053 ) ) ;
#7640 = DIRECTION ( 'NONE',  ( 0.000000000000000000, 0.000000000000000000, -1.000000000000000000 ) ) ;
#7641 = SURFACE_STYLE_USAGE ( .BOTH. , #7785 ) ;
#7642 = CARTESIAN_POINT ( 'NONE',  ( -41.08716857408418122, 108.0000000000001421, 4.165101599090693094E-14 ) ) ;
#7643 = CARTESIAN_POINT ( 'NONE',  ( -4.000000000000000000, 0.3904826640788008341, -1.524659305057739994E-17 ) ) ;
#7644 = CYLINDRICAL_SURFACE ( 'NONE', #3990, 4.999999999999997335 ) ;
#7645 = EDGE_CURVE ( 'NONE', #4939, #5642, #4459, .T. ) ;
#7646 = EDGE_LOOP ( 'NONE', ( #6887, #6585, #1608 ) ) ;
#7647 = ADVANCED_BREP_SHAPE_REPRESENTATION ( '', ( #1247, #1587 ), #4833 ) ;
#7648 = ORIENTED_EDGE ( 'NONE', *, *, #329, .F. ) ;
#7649 = CARTESIAN_POINT ( 'NONE',  ( 29.99999999999997868, 30.00000000000001421, 1.734723475976807094E-15 ) ) ;
#7650 = ORIENTED_EDGE ( 'NONE', *, *, #5815, .F. ) ;
#7651 = ORIENTED_EDGE ( 'NONE', *, *, #5703, .T. ) ;
#7652 = VECTOR ( 'NONE', #4167, 1000.000000000000000 ) ;
#7653 = DIRECTION ( 'NONE',  ( -0.000000000000000000, -1.000000000000000000, -0.000000000000000000 ) ) ;
#7654 = CYLINDRICAL_SURFACE ( 'NONE', #8205, 2.750000000000000000 ) ;
#7655 = CARTESIAN_POINT ( 'NONE',  ( 1.300000000000000044, 0.000000000000000000, 0.000000000000000000 ) ) ;
#7656 = EDGE_CURVE ( 'NONE', #1494, #4585, #5588, .T. ) ;
#7657 = ORIENTED_EDGE ( 'NONE', *, *, #4882, .F. ) ;
#7658 = VERTEX_POINT ( 'NONE', #5823 ) ;
#7659 = ORIENTED_EDGE ( 'NONE', *, *, #3808, .F. ) ;
#7660 = PLANE ( 'NONE',  #245 ) ;
#7661 = CARTESIAN_POINT ( 'NONE',  ( 41.93505285506405045, 87.33493033277945017, 0.5694876689909349476 ) ) ;
#7662 = CARTESIAN_POINT ( 'NONE',  ( 2.500000000000002220, -1.178949249685215417, 2.042000000000002036 ) ) ;
#7663 = CARTESIAN_POINT ( 'NONE',  ( 19.61000000000001720, 2.449293598294707893E-16, -2.000000000000000888 ) ) ;
#7664 = AXIS2_PLACEMENT_3D ( 'NONE', #721, #4339, #90 ) ;
#7665 = PRODUCT_DEFINITION ( 'UNKNOWN', '', #6019, #5323 ) ;
#7666 = EDGE_CURVE ( 'NONE', #2734, #2318, #8181, .T. ) ;
#7667 = FACE_OUTER_BOUND ( 'NONE', #41, .T. ) ;
#7668 = CARTESIAN_POINT ( 'NONE',  ( 39.00000000000003553, 85.00000000000017053, 2.000000000000043077 ) ) ;
#7669 = AXIS2_PLACEMENT_3D ( 'NONE', #7970, #4156, #6106 ) ;
#7670 = DIRECTION ( 'NONE',  ( 0.000000000000000000, 0.000000000000000000, -1.000000000000000000 ) ) ;
#7671 = AXIS2_PLACEMENT_3D ( 'NONE', #4269, #2892, #4891 ) ;
#7672 = CARTESIAN_POINT ( 'NONE',  ( 52.00000000000000000, 7.999999999999996447, 11.99999999999998934 ) ) ;
#7673 = VECTOR ( 'NONE', #4779, 1000.000000000000000 ) ;
#7674 = VERTEX_POINT ( 'NONE', #2772 ) ;
#7675 = DIRECTION ( 'NONE',  ( 1.000000000000000000, 0.000000000000000000, 0.000000000000000000 ) ) ;
#7676 = CIRCLE ( 'NONE', #5423, 1.599999999999998979 ) ;
#7677 = CARTESIAN_POINT ( 'NONE',  ( 5.860087342385653250E-15, 38.99999999999999289, 0.000000000000000000 ) ) ;
#7678 = VECTOR ( 'NONE', #6679, 1000.000000000000227 ) ;
#7679 = CARTESIAN_POINT ( 'NONE',  ( 1.214306433183764966E-14, 4.618802153517020059, -2.700000000000000178 ) ) ;
#7680 = CONICAL_SURFACE ( 'NONE', #6216, 2.060000000000000941, 0.9599310885968777018 ) ;
#7681 = VECTOR ( 'NONE', #3711, 1000.000000000000114 ) ;
#7682 = LINE ( 'NONE', #7097, #8058 ) ;
#7683 =( NAMED_UNIT ( * ) PLANE_ANGLE_UNIT ( ) SI_UNIT ( $, .RADIAN. ) );
#7684 = AXIS2_PLACEMENT_3D ( 'NONE', #3021, #4355, #6224 ) ;
#7685 = ORIENTED_EDGE ( 'NONE', *, *, #4147, .F. ) ;
#7686 = EDGE_CURVE ( 'NONE', #7574, #2944, #2505, .T. ) ;
#7687 = AXIS2_PLACEMENT_3D ( 'NONE', #1813, #8151, #5509 ) ;
#7688 = ORIENTED_EDGE ( 'NONE', *, *, #4258, .F. ) ;
#7689 = MECHANICAL_DESIGN_GEOMETRIC_PRESENTATION_REPRESENTATION (  '', ( #2652 ), #4966 ) ;
#7690 = CARTESIAN_POINT ( 'NONE',  ( 41.99951245237345177, 84.76684522874218430, 2.391513083590206534 ) ) ;
#7691 = ORIENTED_EDGE ( 'NONE', *, *, #1097, .F. ) ;
#7692 = EDGE_CURVE ( 'NONE', #3432, #2115, #7703, .T. ) ;
#7693 = ORIENTED_EDGE ( 'NONE', *, *, #1846, .F. ) ;
#7694 = VECTOR ( 'NONE', #5213, 1000.000000000000114 ) ;
#7695 = DIRECTION ( 'NONE',  ( 0.000000000000000000, 1.000000000000000000, 0.000000000000000000 ) ) ;
#7696 = DIRECTION ( 'NONE',  ( 0.000000000000000000, 0.000000000000000000, 1.000000000000000000 ) ) ;
#7697 = DIRECTION ( 'NONE',  ( 1.000000000000000000, 0.000000000000000000, 0.000000000000000000 ) ) ;
#7698 = AXIS2_PLACEMENT_3D ( 'NONE', #3463, #7270, #7741 ) ;
#7699 = COLOUR_RGB ( '', 0.08235294, 0.09019608, 0.10196078) ;
#7700 = ORIENTED_EDGE ( 'NONE', *, *, #2801, .T. ) ;
#7701 = ORIENTED_EDGE ( 'NONE', *, *, #1009, .T. ) ;
#7702 = ORIENTED_EDGE ( 'NONE', *, *, #1957, .T. ) ;
#7703 = CIRCLE ( 'NONE', #4784, 4.999999999999993783 ) ;
#7704 = DIRECTION ( 'NONE',  ( -1.000000000000000000, 0.000000000000000000, 0.000000000000000000 ) ) ;
#7705 = CARTESIAN_POINT ( 'NONE',  ( 41.95747712235107940, 86.89089932782653136, -1.483502059618200253 ) ) ;
#7706 = CARTESIAN_POINT ( 'NONE',  ( 0.000000000000000000, 0.000000000000000000, -2.700000000000001066 ) ) ;
#7707 =( LENGTH_UNIT ( ) NAMED_UNIT ( * ) SI_UNIT ( .MILLI., .METRE. ) );
#7708 = AXIS2_PLACEMENT_3D ( 'NONE', #5340, #6528, #208 ) ;
#7709 = CARTESIAN_POINT ( 'NONE',  ( -3.698018259095727789, -5.947912380466928717, 8.009454966680493726 ) ) ;
#7710 = EDGE_CURVE ( 'NONE', #5372, #792, #2532, .T. ) ;
#7711 = EDGE_CURVE ( 'NONE', #2320, #8100, #5317, .T. ) ;
#7712 = DIRECTION ( 'NONE',  ( -0.000000000000000000, -0.000000000000000000, -1.000000000000000000 ) ) ;
#7713 = LINE ( 'NONE', #2572, #661 ) ;
#7714 = DIRECTION ( 'NONE',  ( 0.000000000000000000, 0.000000000000000000, -1.000000000000000000 ) ) ;
#7715 = FACE_OUTER_BOUND ( 'NONE', #5268, .T. ) ;
#7716 = CYLINDRICAL_SURFACE ( 'NONE', #1964, 2.000000000000000888 ) ;
#7717 = EDGE_LOOP ( 'NONE', ( #3956, #3788 ) ) ;
#7718 = CARTESIAN_POINT ( 'NONE',  ( 2.000000000000000000, 1.773042676681340968, -2.276824562219559311E-15 ) ) ;
#7719 = DIRECTION ( 'NONE',  ( 0.000000000000000000, 0.000000000000000000, -1.000000000000000000 ) ) ;
#7720 = DIRECTION ( 'NONE',  ( 0.000000000000000000, 0.000000000000000000, -1.000000000000000000 ) ) ;
#7721 = LINE ( 'NONE', #888, #6470 ) ;
#7722 = CARTESIAN_POINT ( 'NONE',  ( 2.000000000000000000, -1.773042676681340524, 1.734723475976807094E-15 ) ) ;
#7723 = AXIS2_PLACEMENT_3D ( 'NONE', #2188, #7249, #2854 ) ;
#7724 = ADVANCED_FACE ( 'NONE', ( #586 ), #7654, .T. ) ;
#7725 = ORIENTED_EDGE ( 'NONE', *, *, #6480, .F. ) ;
#7726 = CARTESIAN_POINT ( 'NONE',  ( -3.673643420401911719, -2.497823135841289677, -2.451519936624989349 ) ) ;
#7727 = EDGE_CURVE ( 'NONE', #2205, #8175, #7578, .T. ) ;
#7728 = ORIENTED_EDGE ( 'NONE', *, *, #3565, .T. ) ;
#7729 = CARTESIAN_POINT ( 'NONE',  ( 42.00000000000003553, 85.00000000000049738, 2.399999999999971934 ) ) ;
#7730 = VERTEX_POINT ( 'NONE', #744 ) ;
#7731 = ORIENTED_EDGE ( 'NONE', *, *, #6949, .T. ) ;
#7732 = CARTESIAN_POINT ( 'NONE',  ( 0.1999999999999987899, 0.000000000000000000, 3.299999999999999822 ) ) ;
#7733 = EDGE_CURVE ( 'NONE', #8077, #2944, #4421, .T. ) ;
#7734 = LINE ( 'NONE', #2707, #6351 ) ;
#7735 = DIRECTION ( 'NONE',  ( 1.363075293218192124E-18, -1.363075293218191931E-18, 1.000000000000000000 ) ) ;
#7736 = APPLICATION_CONTEXT ( 'automotive_design' ) ;
#7737 = EDGE_CURVE ( 'NONE', #2258, #7104, #3588, .T. ) ;
#7738 = ORIENTED_EDGE ( 'NONE', *, *, #4117, .T. ) ;
#7739 = ORIENTED_EDGE ( 'NONE', *, *, #7346, .F. ) ;
#7740 = ORIENTED_EDGE ( 'NONE', *, *, #2683, .T. ) ;
#7741 = DIRECTION ( 'NONE',  ( -1.000000000000000000, -2.775557561562890365E-16, 1.734723475976806478E-17 ) ) ;
#7742 = CARTESIAN_POINT ( 'NONE',  ( 4.000000000000001776, 0.000000000000000000, -2.200000000000001066 ) ) ;
#7743 = CARTESIAN_POINT ( 'NONE',  ( 50.00000000000003553, 85.00000000000012790, 5.000000000000045297 ) ) ;
#7744 =( NAMED_UNIT ( * ) SI_UNIT ( $, .STERADIAN. ) SOLID_ANGLE_UNIT ( ) );
#7745 = STYLED_ITEM ( 'NONE', ( #998 ), #9 ) ;
#7746 = DIRECTION ( 'NONE',  ( 2.168404344971008621E-16, -1.000000000000000000, 0.000000000000000000 ) ) ;
#7747 = DIRECTION ( 'NONE',  ( 0.000000000000000000, 0.000000000000000000, 1.000000000000000000 ) ) ;
#7748 = FACE_OUTER_BOUND ( 'NONE', #364, .T. ) ;
#7749 = FACE_OUTER_BOUND ( 'NONE', #5494, .T. ) ;
#7750 = CIRCLE ( 'NONE', #7217, 2.041999999999999815 ) ;
#7751 = ORIENTED_EDGE ( 'NONE', *, *, #2862, .T. ) ;
#7752 = DIRECTION ( 'NONE',  ( 0.000000000000000000, 0.000000000000000000, -1.000000000000000000 ) ) ;
#7753 = CARTESIAN_POINT ( 'NONE',  ( -7.502679033599690683E-14, -4.618802153517020059, -2.342734410091827701 ) ) ;
#7754 = DIRECTION ( 'NONE',  ( -1.000000000000000000, 0.000000000000000000, 2.065146995210483462E-17 ) ) ;
#7755 = EDGE_CURVE ( 'NONE', #7485, #1738, #711, .T. ) ;
#7756 = ORIENTED_EDGE ( 'NONE', *, *, #7037, .F. ) ;
#7757 = DIRECTION ( 'NONE',  ( 0.000000000000000000, -1.000000000000000000, 1.287488025362403787E-15 ) ) ;
#7758 = ORIENTED_EDGE ( 'NONE', *, *, #3030, .F. ) ;
#7759 = ORIENTED_EDGE ( 'NONE', *, *, #4064, .F. ) ;
#7760 = LINE ( 'NONE', #2082, #6574 ) ;
#7761 = ADVANCED_FACE ( 'NONE', ( #1301 ), #6372, .F. ) ;
#7762 = CARTESIAN_POINT ( 'NONE',  ( 58.00000000000000000, 8.000000000000000000, 0.000000000000000000 ) ) ;
#7763 = EDGE_CURVE ( 'NONE', #7076, #3705, #1349, .T. ) ;
#7764 = EDGE_CURVE ( 'NONE', #3149, #2847, #7039, .T. ) ;
#7765 = DIRECTION ( 'NONE',  ( 0.000000000000000000, -0.8660254037844391517, -0.4999999999999991118 ) ) ;
#7766 = SHAPE_DEFINITION_REPRESENTATION ( #4313, #6987 ) ;
#7767 = ORIENTED_EDGE ( 'NONE', *, *, #5596, .F. ) ;
#7768 = EDGE_LOOP ( 'NONE', ( #1265, #6097, #4772 ) ) ;
#7769 = CIRCLE ( 'NONE', #4193, 1.250000000000001110 ) ;
#7770 = ORIENTED_EDGE ( 'NONE', *, *, #148, .T. ) ;
#7771 = DIRECTION ( 'NONE',  ( 1.000000000000000000, 0.000000000000000000, 0.000000000000000000 ) ) ;
#7772 = CARTESIAN_POINT ( 'NONE',  ( -42.00000000000000711, 85.00000000000046896, 2.399999999999971045 ) ) ;
#7773 = CARTESIAN_POINT ( 'NONE',  ( -31.74999999999994316, 0.000000000000000000, 4.250000000000000000 ) ) ;
#7774 = AXIS2_PLACEMENT_3D ( 'NONE', #4605, #7013, #7129 ) ;
#7775 = CIRCLE ( 'NONE', #1422, 0.1000000000000000472 ) ;
#7776 = EDGE_CURVE ( 'NONE', #7219, #5215, #5789, .T. ) ;
#7777 = DIRECTION ( 'NONE',  ( -1.000000000000000000, -0.000000000000000000, -0.000000000000000000 ) ) ;
#7778 = CARTESIAN_POINT ( 'NONE',  ( -32.64999999999999147, 30.00000000000000711, 4.599999999999997868 ) ) ;
#7779 = DIRECTION ( 'NONE',  ( -1.000000000000000000, 0.000000000000000000, 0.000000000000000000 ) ) ;
#7780 = CARTESIAN_POINT ( 'NONE',  ( -31.74999999999994316, 0.000000000000000000, 2.500000000000000444 ) ) ;
#7781 = CARTESIAN_POINT ( 'NONE',  ( 50.00000000000000000, -10.00000000000000000, 0.000000000000000000 ) ) ;
#7782 = EDGE_CURVE ( 'NONE', #792, #5372, #6762, .T. ) ;
#7783 = VERTEX_POINT ( 'NONE', #7212 ) ;
#7784 = DIRECTION ( 'NONE',  ( -1.000000000000000000, 0.000000000000000000, 0.000000000000000000 ) ) ;
#7785 = SURFACE_SIDE_STYLE ('',( #2581 ) ) ;
#7786 = CARTESIAN_POINT ( 'NONE',  ( -31.74999999999995737, 0.000000000000000000, 2.000000000000000888 ) ) ;
#7787 = AXIS2_PLACEMENT_3D ( 'NONE', #639, #1945, #1863 ) ;
#7788 = CARTESIAN_POINT ( 'NONE',  ( 57.99999999999999289, -8.000000000000003553, 11.99999999999998934 ) ) ;
#7789 = DIRECTION ( 'NONE',  ( -0.000000000000000000, -0.000000000000000000, 1.000000000000000000 ) ) ;
#7790 = ORIENTED_EDGE ( 'NONE', *, *, #2561, .F. ) ;
#7791 = CARTESIAN_POINT ( 'NONE',  ( 4.199999999999995737, 0.000000000000000000, 2.000000000000000888 ) ) ;
#7792 = UNCERTAINTY_MEASURE_WITH_UNIT (LENGTH_MEASURE( 1.000000000000000082E-05 ), #6154, 'distance_accuracy_value', 'NONE');
#7793 =( GEOMETRIC_REPRESENTATION_CONTEXT ( 3 ) GLOBAL_UNCERTAINTY_ASSIGNED_CONTEXT ( ( #383 ) ) GLOBAL_UNIT_ASSIGNED_CONTEXT ( ( #5531, #7919, #409 ) ) REPRESENTATION_CONTEXT ( 'NONE', 'WORKASPACE' ) );
#7794 = VERTEX_POINT ( 'NONE', #3480 ) ;
#7795 = EDGE_CURVE ( 'NONE', #7441, #7139, #7956, .T. ) ;
#7796 = ORIENTED_EDGE ( 'NONE', *, *, #1655, .F. ) ;
#7797 = CLOSED_SHELL ( 'NONE', ( #963, #6970, #4818, #2151, #1585, #2073, #7882, #2958, #1315, #1008, #5375, #4452, #7819, #2877, #4789, #2682, #7149, #1999, #5902, #836, #5139, #4274, #4276, #6685, #5526, #2232, #3200, #454, #3406, #8145, #4850, #6455, #2042 ) ) ;
#7798 = VECTOR ( 'NONE', #3910, 1000.000000000000114 ) ;
#7799 = AXIS2_PLACEMENT_3D ( 'NONE', #2503, #7653, #710 ) ;
#7800 = CARTESIAN_POINT ( 'NONE',  ( -29.99999999999999289, 30.00000000000000711, 10.00000000000000000 ) ) ;
#7801 = EDGE_CURVE ( 'NONE', #6597, #7134, #5518, .T. ) ;
#7802 = CARTESIAN_POINT ( 'NONE',  ( 5.000000000000015099, 0.000000000000000000, 0.000000000000000000 ) ) ;
#7803 = FACE_OUTER_BOUND ( 'NONE', #7768, .T. ) ;
#7804 = APPLICATION_PROTOCOL_DEFINITION ( 'draft international standard', 'automotive_design', 1998, #927 ) ;
#7805 = AXIS2_PLACEMENT_3D ( 'NONE', #7258, #1578, #4114 ) ;
#7806 = VECTOR ( 'NONE', #6423, 1000.000000000000227 ) ;
#7807 = AXIS2_PLACEMENT_3D ( 'NONE', #6091, #4103, #8032 ) ;
#7808 = EDGE_CURVE ( 'NONE', #6822, #2407, #4120, .T. ) ;
#7809 = ORIENTED_EDGE ( 'NONE', *, *, #187, .T. ) ;
#7810 = EDGE_LOOP ( 'NONE', ( #5396, #828 ) ) ;
#7811 = EDGE_LOOP ( 'NONE', ( #7170, #5893, #2268, #6781, #5332, #3819 ) ) ;
#7812 = CIRCLE ( 'NONE', #4243, 2.500000000000002220 ) ;
#7813 = DIRECTION ( 'NONE',  ( -0.000000000000000000, -0.000000000000000000, 1.000000000000000000 ) ) ;
#7814 = PLANE ( 'NONE',  #6235 ) ;
#7815 = AXIS2_PLACEMENT_3D ( 'NONE', #2030, #1320, #7747 ) ;
#7816 =( LENGTH_UNIT ( ) NAMED_UNIT ( * ) SI_UNIT ( .MILLI., .METRE. ) );
#7817 = ORIENTED_EDGE ( 'NONE', *, *, #2612, .T. ) ;
#7818 = FACE_OUTER_BOUND ( 'NONE', #1800, .T. ) ;
#7819 = ADVANCED_FACE ( 'NONE', ( #4808 ), #4182, .F. ) ;
#7821 = EDGE_CURVE ( 'NONE', #4997, #1429, #2273, .T. ) ;
#7820 = AXIS2_PLACEMENT_3D ( 'NONE', #3039, #6856, #1166 ) ;
#7822 = CARTESIAN_POINT ( 'NONE',  ( 7.000000000000000000, 8.572527594031473190E-16, 18.00000000000000355 ) ) ;
#7823 = CARTESIAN_POINT ( 'NONE',  ( 0.000000000000000000, 0.000000000000000000, -2.700000000000000178 ) ) ;
#7824 = VECTOR ( 'NONE', #8116, 1000.000000000000000 ) ;
#7825 =( NAMED_UNIT ( * ) PLANE_ANGLE_UNIT ( ) SI_UNIT ( $, .RADIAN. ) );
#7826 = EDGE_CURVE ( 'NONE', #6759, #1110, #4370, .T. ) ;
#7827 = FACE_BOUND ( 'NONE', #6620, .T. ) ;
#7828 = CIRCLE ( 'NONE', #7046, 7.000000000000000000 ) ;
#7829 = DIRECTION ( 'NONE',  ( 1.000000000000000000, -0.000000000000000000, -0.000000000000000000 ) ) ;
#7830 = ORIENTED_EDGE ( 'NONE', *, *, #3583, .T. ) ;
#7831 = CARTESIAN_POINT ( 'NONE',  ( 1.300000000000000044, -0.7390083445627200209, 1.280000000000001137 ) ) ;
#7832 = DIRECTION ( 'NONE',  ( 0.000000000000000000, 0.000000000000000000, -1.000000000000000000 ) ) ;
#7833 = DIRECTION ( 'NONE',  ( 1.000000000000000000, 0.000000000000000000, 0.000000000000000000 ) ) ;
#7834 = DIRECTION ( 'NONE',  ( -1.000000000000000000, 0.000000000000000000, 0.000000000000000000 ) ) ;
#7835 = DIRECTION ( 'NONE',  ( -0.5000000000000034417, 1.060575238724904696E-16, -0.8660254037844367092 ) ) ;
#7836 = CARTESIAN_POINT ( 'NONE',  ( -49.97873132679185915, 83.53599209938492720, -1.908173386893793566 ) ) ;
#7837 = PLANE ( 'NONE',  #7723 ) ;
#7838 = EDGE_LOOP ( 'NONE', ( #4067, #981, #4542, #2995 ) ) ;
#7839 = DIRECTION ( 'NONE',  ( -1.000000000000000000, -1.502586498047605218E-16, 1.238733049487200360E-17 ) ) ;
#7840 = EDGE_LOOP ( 'NONE', ( #7960, #1599, #7909, #7934 ) ) ;
#7841 = EDGE_LOOP ( 'NONE', ( #6546, #3412, #3411, #4698 ) ) ;
#7842 = CARTESIAN_POINT ( 'NONE',  ( 1.660531772554324492, -3.660093687634889736, -2.699999999999979305 ) ) ;
#7843 = FACE_OUTER_BOUND ( 'NONE', #5746, .T. ) ;
#7844 = DIRECTION ( 'NONE',  ( -0.000000000000000000, -0.000000000000000000, 1.000000000000000000 ) ) ;
#7845 = DIRECTION ( 'NONE',  ( 1.412205397084881070E-17, -2.775557561562891967E-17, -1.000000000000000000 ) ) ;
#7846 = CONTEXT_DEPENDENT_SHAPE_REPRESENTATION ( #3067, #6969 ) ;
#7847 = EDGE_CURVE ( 'NONE', #4432, #3047, #4632, .T. ) ;
#7848 = EDGE_CURVE ( 'NONE', #7139, #6188, #433, .T. ) ;
#7849 = ADVANCED_FACE ( 'NONE', ( #3439 ), #3519, .F. ) ;
#7850 = AXIS2_PLACEMENT_3D ( 'NONE', #5574, #3791, #1922 ) ;
#7851 = EDGE_LOOP ( 'NONE', ( #6209, #1504, #5897, #199 ) ) ;
#7852 = ORIENTED_EDGE ( 'NONE', *, *, #6936, .F. ) ;
#7853 = ORIENTED_EDGE ( 'NONE', *, *, #2727, .F. ) ;
#7854 = FACE_OUTER_BOUND ( 'NONE', #2308, .T. ) ;
#7855 = CARTESIAN_POINT ( 'NONE',  ( 1.274374112546295138E-14, 85.00000000000017053, 2.000000000000043521 ) ) ;
#7856 = CARTESIAN_POINT ( 'NONE',  ( 0.2500000000000002220, 0.000000000000000000, 2.081668171172168513E-14 ) ) ;
#7857 = CARTESIAN_POINT ( 'NONE',  ( 60.00000000000000711, 9.534646258076108189E-15, 56.64999999999996305 ) ) ;
#7858 = DIRECTION ( 'NONE',  ( 0.000000000000000000, 1.000000000000000000, -0.000000000000000000 ) ) ;
#7859 = EDGE_CURVE ( 'NONE', #7134, #5096, #4720, .T. ) ;
#7860 = EDGE_CURVE ( 'NONE', #5018, #6188, #7247, .T. ) ;
#7861 = LINE ( 'NONE', #4748, #7155 ) ;
#7862 = DIRECTION ( 'NONE',  ( 0.000000000000000000, 0.000000000000000000, 1.000000000000000000 ) ) ;
#7863 = DIRECTION ( 'NONE',  ( 0.000000000000000000, 0.000000000000000000, 1.000000000000000000 ) ) ;
#7864 = ORIENTED_EDGE ( 'NONE', *, *, #2182, .T. ) ;
#7865 = EDGE_LOOP ( 'NONE', ( #7878, #6121, #1080, #7127 ) ) ;
#7866 = DIRECTION ( 'NONE',  ( 0.8660254037844372643, 0.5000000000000026645, 0.000000000000000000 ) ) ;
#7867 = CARTESIAN_POINT ( 'NONE',  ( -50.00000000000000711, 85.00000000000009948, -5.000000000000005329 ) ) ;
#7868 = LINE ( 'NONE', #7905, #2361 ) ;
#7869 = DIRECTION ( 'NONE',  ( 0.000000000000000000, 0.000000000000000000, 1.000000000000000000 ) ) ;
#7870 = SHAPE_REPRESENTATION ( 'socket head cap screw_iso_ISO 4762 M4 x 20 - 20N', ( #1587 ), #4833 ) ;
#7871 = CARTESIAN_POINT ( 'NONE',  ( -49.96363327394940512, 83.09135878423528254, -1.463402463582062829 ) ) ;
#7872 = FACE_OUTER_BOUND ( 'NONE', #376, .T. ) ;
#7873 = VERTEX_POINT ( 'NONE', #1565 ) ;
#7874 = DIRECTION ( 'NONE',  ( -1.000000000000000000, 0.000000000000000000, 0.000000000000000000 ) ) ;
#7875 = AXIS2_PLACEMENT_3D ( 'NONE', #4099, #3389, #7866 ) ;
#7876 = ORIENTED_EDGE ( 'NONE', *, *, #687, .T. ) ;
#7877 = APPLICATION_CONTEXT ( 'automotive_design' ) ;
#7878 = ORIENTED_EDGE ( 'NONE', *, *, #2648, .F. ) ;
#7879 = CARTESIAN_POINT ( 'NONE',  ( 2.000000000000010658, -3.464101615137748169, -2.700000000000001066 ) ) ;
#7880 = DIRECTION ( 'NONE',  ( -1.000000000000000000, -0.000000000000000000, -0.000000000000000000 ) ) ;
#7881 = CARTESIAN_POINT ( 'NONE',  ( -1.599999999999992983, 37.49999999999999289, 4.000000000000000000 ) ) ;
#7882 = ADVANCED_FACE ( 'NONE', ( #4140 ), #6004, .T. ) ;
#7883 = DIRECTION ( 'NONE',  ( 0.000000000000000000, -1.000000000000000000, 0.000000000000000000 ) ) ;
#7884 = CARTESIAN_POINT ( 'NONE',  ( 40.00000000000000711, -39.99999999999999289, 10.00000000000000000 ) ) ;
#7885 = ORIENTED_EDGE ( 'NONE', *, *, #1940, .T. ) ;
#7886 = ORIENTED_EDGE ( 'NONE', *, *, #6126, .F. ) ;
#7887 = EDGE_LOOP ( 'NONE', ( #3525, #6914 ) ) ;
#7888 = FACE_BOUND ( 'NONE', #1941, .T. ) ;
#7889 = CARTESIAN_POINT ( 'NONE',  ( 1.300000000000000044, 1.478016689125442484, -1.626303258728256651E-15 ) ) ;
#7890 = CYLINDRICAL_SURFACE ( 'NONE', #2236, 50.00000000000002132 ) ;
#7891 = SURFACE_SIDE_STYLE ('',( #1511 ) ) ;
#7892 = LINE ( 'NONE', #6656, #1471 ) ;
#7893 = CARTESIAN_POINT ( 'NONE',  ( -1.321505333908964186, 3.855830693249143071, -0.03421028094653202900 ) ) ;
#7894 = CARTESIAN_POINT ( 'NONE',  ( 2.000000000000000000, 0.000000000000000000, 0.000000000000000000 ) ) ;
#7895 = VECTOR ( 'NONE', #7359, 1000.000000000000000 ) ;
#7896 = SHAPE_REPRESENTATION_RELATIONSHIP ( 'NONE' , 'NONE' ,  #2475, #6832 ) ;
#7897 = CYLINDRICAL_SURFACE ( 'NONE', #2799, 1.500000000000000222 ) ;
#7898 = CARTESIAN_POINT ( 'NONE',  ( -34.99999999999999289, 30.00000000000000711, 4.599999999999997868 ) ) ;
#7899 = PRODUCT_DEFINITION ( 'UNKNOWN', '', #2697, #3756 ) ;
#7900 = ORIENTED_EDGE ( 'NONE', *, *, #6539, .F. ) ;
#7901 = ORIENTED_EDGE ( 'NONE', *, *, #2520, .F. ) ;
#7902 = CARTESIAN_POINT ( 'NONE',  ( 0.000000000000000000, 4.163799117101000559E-16, -3.299999999999999822 ) ) ;
#7903 = DIRECTION ( 'NONE',  ( 1.000000000000000000, 0.000000000000000000, 0.000000000000000000 ) ) ;
#7904 = DIRECTION ( 'NONE',  ( -1.000000000000000000, -0.000000000000000000, -0.000000000000000000 ) ) ;
#7905 = CARTESIAN_POINT ( 'NONE',  ( 60.00000000000000711, -10.00000000000000000, 60.00000000000000000 ) ) ;
#7906 = CARTESIAN_POINT ( 'NONE',  ( 0.1999999999999987899, 0.000000000000000000, 3.500000000000000000 ) ) ;
#7907 = CARTESIAN_POINT ( 'NONE',  ( 4.199999999999995737, 0.000000000000000000, 0.000000000000000000 ) ) ;
#7908 = DIRECTION ( 'NONE',  ( 0.000000000000000000, 0.000000000000000000, 1.000000000000000000 ) ) ;
#7909 = ORIENTED_EDGE ( 'NONE', *, *, #5485, .T. ) ;
#7910 = DIRECTION ( 'NONE',  ( -0.000000000000000000, -0.000000000000000000, 1.000000000000000000 ) ) ;
#7911 = ORIENTED_EDGE ( 'NONE', *, *, #7434, .F. ) ;
#7912 = ORIENTED_EDGE ( 'NONE', *, *, #7755, .F. ) ;
#7913 = VECTOR ( 'NONE', #3894, 1000.000000000000000 ) ;
#7914 = CARTESIAN_POINT ( 'NONE',  ( 57.99999999999999289, -8.000000000000003553, 19.99999999999998934 ) ) ;
#7915 = DIRECTION ( 'NONE',  ( 0.000000000000000000, 0.4999999999999990008, -0.8660254037844391517 ) ) ;
#7916 = CARTESIAN_POINT ( 'NONE',  ( 4.000000000000003553, -0.7779732554280839318, -2.666455648918319987 ) ) ;
#7917 = AXIS2_PLACEMENT_3D ( 'NONE', #4982, #6878, #520 ) ;
#7918 = CARTESIAN_POINT ( 'NONE',  ( -6.773732078532765932, 1.824713701299700563, 8.031803308098282912 ) ) ;
#7919 =( NAMED_UNIT ( * ) PLANE_ANGLE_UNIT ( ) SI_UNIT ( $, .RADIAN. ) );
#7920 = APPLICATION_PROTOCOL_DEFINITION ( 'draft international standard', 'automotive_design', 1998, #6602 ) ;
#7921 = VECTOR ( 'NONE', #3834, 1000.000000000000114 ) ;
#7922 = EDGE_CURVE ( 'NONE', #2129, #3337, #1860, .T. ) ;
#7923 = CIRCLE ( 'NONE', #3422, 4.999999999999993783 ) ;
#7924 = VECTOR ( 'NONE', #8171, 1000.000000000000000 ) ;
#7925 = ORIENTED_EDGE ( 'NONE', *, *, #1655, .T. ) ;
#7926 = EDGE_LOOP ( 'NONE', ( #492, #908, #1503, #630 ) ) ;
#7927 = VERTEX_POINT ( 'NONE', #7906 ) ;
#7928 = DIRECTION ( 'NONE',  ( 0.000000000000000000, 1.000000000000000000, 0.000000000000000000 ) ) ;
#7929 = CARTESIAN_POINT ( 'NONE',  ( 0.1999999999999987899, 4.041334437186265510E-16, -3.299999999999999822 ) ) ;
#7930 = CARTESIAN_POINT ( 'NONE',  ( 2.000000000000000000, -0.8865213383406685965, 1.535500000000000531 ) ) ;
#7931 = AXIS2_PLACEMENT_3D ( 'NONE', #7965, #7880, #4905 ) ;
#7932 = VECTOR ( 'NONE', #5803, 1000.000000000000000 ) ;
#7933 = CIRCLE ( 'NONE', #116, 1.249999999999998002 ) ;
#7934 = ORIENTED_EDGE ( 'NONE', *, *, #3102, .F. ) ;
#7935 = CYLINDRICAL_SURFACE ( 'NONE', #7112, 42.00000000000002132 ) ;
#7936 = VECTOR ( 'NONE', #2990, 1000.000000000000000 ) ;
#7937 = CARTESIAN_POINT ( 'NONE',  ( -0.3263565795980840067, 4.430380094434251959, -0.2484800633750075816 ) ) ;
#7938 = DIRECTION ( 'NONE',  ( -1.000000000000000000, 0.000000000000000000, 0.000000000000000000 ) ) ;
#7939 = VECTOR ( 'NONE', #672, 1000.000000000000227 ) ;
#7940 = AXIS2_PLACEMENT_3D ( 'NONE', #5537, #7928, #4919 ) ;
#7941 = DIRECTION ( 'NONE',  ( 0.000000000000000000, -1.000000000000000000, 1.026972870230479989E-15 ) ) ;
#7942 = UNCERTAINTY_MEASURE_WITH_UNIT (LENGTH_MEASURE( 1.000000000000000082E-05 ), #5802, 'distance_accuracy_value', 'NONE');
#7943 = EDGE_CURVE ( 'NONE', #8142, #3962, #1326, .T. ) ;
#7944 = CIRCLE ( 'NONE', #781, 3.999999999999999112 ) ;
#7945 = VECTOR ( 'NONE', #3560, 1000.000000000000000 ) ;
#7946 = EDGE_CURVE ( 'NONE', #2115, #2558, #7992, .T. ) ;
#7947 = CARTESIAN_POINT ( 'NONE',  ( 7.000000000000000000, 0.4570009800896051022, 8.033969604113655905 ) ) ;
#7948 = EDGE_CURVE ( 'NONE', #2820, #3778, #7298, .T. ) ;
#7949 = VERTEX_POINT ( 'NONE', #978 ) ;
#7950 = ORIENTED_EDGE ( 'NONE', *, *, #5989, .F. ) ;
#7951 = PLANE ( 'NONE',  #843 ) ;
#7952 = CIRCLE ( 'NONE', #4525, 0.2000000000000000944 ) ;
#7953 = DIRECTION ( 'NONE',  ( 0.000000000000000000, 0.000000000000000000, 1.000000000000000000 ) ) ;
#7954 = CARTESIAN_POINT ( 'NONE',  ( -58.00000000000006395, 7.999999999999996447, 19.99999999999998934 ) ) ;
#7955 = DIRECTION ( 'NONE',  ( 0.000000000000000000, -1.000000000000000000, 0.000000000000000000 ) ) ;
#7956 = LINE ( 'NONE', #1017, #7294 ) ;
#7957 = CARTESIAN_POINT ( 'NONE',  ( -50.00000000000000711, 85.00000000000009948, -2.399999999999999467 ) ) ;
#7958 = AXIS2_PLACEMENT_3D ( 'NONE', #5264, #5424, #6502 ) ;
#7959 = DIRECTION ( 'NONE',  ( -1.000000000000000000, 0.000000000000000000, 0.000000000000000000 ) ) ;
#7960 = ORIENTED_EDGE ( 'NONE', *, *, #7341, .F. ) ;
#7961 = DIRECTION ( 'NONE',  ( 0.000000000000000000, -0.000000000000000000, 1.000000000000000000 ) ) ;
#7962 = ORIENTED_EDGE ( 'NONE', *, *, #5528, .F. ) ;
#7963 = ORIENTED_EDGE ( 'NONE', *, *, #3147, .T. ) ;
#7964 = PLANE ( 'NONE',  #7684 ) ;
#7965 = CARTESIAN_POINT ( 'NONE',  ( 2.000000000000000000, 0.000000000000000000, 0.000000000000000000 ) ) ;
#7966 = CYLINDRICAL_SURFACE ( 'NONE', #1906, 4.999999999999993783 ) ;
#7967 = B_SPLINE_CURVE_WITH_KNOTS ( 'NONE', 3,
 ( #7525, #626, #6409, #1259, #5626, #44 ),
 .UNSPECIFIED., .F., .F.,
 ( 4, 2, 4 ),
 ( 0.01361260127035726804, 0.01431046602193920651, 0.01500833077352114499 ),
 .UNSPECIFIED. ) ;
#7968 = CARTESIAN_POINT ( 'NONE',  ( 2.000000000000000000, 1.329782007511006725, 0.7677499999999987113 ) ) ;
#7969 = ADVANCED_FACE ( 'NONE', ( #6044 ), #3978, .F. ) ;
#7970 = CARTESIAN_POINT ( 'NONE',  ( 0.2500000000000002220, 0.000000000000000000, 2.081668171172168513E-14 ) ) ;
#7971 = ORIENTED_EDGE ( 'NONE', *, *, #904, .T. ) ;
#7972 = ORIENTED_EDGE ( 'NONE', *, *, #3294, .F. ) ;
#7973 = ORIENTED_EDGE ( 'NONE', *, *, #2709, .T. ) ;
#7974 = EDGE_CURVE ( 'NONE', #4662, #4304, #1721, .T. ) ;
#7975 = FACE_OUTER_BOUND ( 'NONE', #2356, .T. ) ;
#7976 = LINE ( 'NONE', #415, #6214 ) ;
#7977 = ADVANCED_FACE ( 'NONE', ( #5021 ), #1870, .F. ) ;
#7978 = AXIS2_PLACEMENT_3D ( 'NONE', #4811, #4062, #6631 ) ;
#7979 = ORIENTED_EDGE ( 'NONE', *, *, #7711, .F. ) ;
#7980 = DIRECTION ( 'NONE',  ( -1.000000000000000000, 0.000000000000000000, 0.000000000000000000 ) ) ;
#7981 = EDGE_LOOP ( 'NONE', ( #3343, #4287, #3356, #822, #4759 ) ) ;
#7982 = DIRECTION ( 'NONE',  ( -0.000000000000000000, -1.000000000000000000, -0.000000000000000000 ) ) ;
#7983 = CARTESIAN_POINT ( 'NONE',  ( 0.000000000000000000, 0.000000000000000000, 0.000000000000000000 ) ) ;
#7984 = EDGE_CURVE ( 'NONE', #7025, #8184, #5571, .T. ) ;
#7985 = DIRECTION ( 'NONE',  ( 0.000000000000000000, 0.000000000000000000, 1.000000000000000000 ) ) ;
#7986 = CARTESIAN_POINT ( 'NONE',  ( 4.620169681576417275, 5.263757874614205079, 8.014776054765157198 ) ) ;
#7987 = ORIENTED_EDGE ( 'NONE', *, *, #2171, .T. ) ;
#7988 = ORIENTED_EDGE ( 'NONE', *, *, #342, .F. ) ;
#7989 = DIRECTION ( 'NONE',  ( -1.000000000000000000, 0.000000000000000000, 0.000000000000000000 ) ) ;
#7990 = LINE ( 'NONE', #6088, #6346 ) ;
#7991 = CARTESIAN_POINT ( 'NONE',  ( 5.930697612239895941E-15, 38.99999999999999289, -4.999999999999990230 ) ) ;
#7992 = LINE ( 'NONE', #2225, #4235 ) ;
#7993 = FACE_OUTER_BOUND ( 'NONE', #2300, .T. ) ;
#7994 = COLOUR_RGB ( '', 0.31764706, 0.68627451, 0.89019608) ;
#7995 = CYLINDRICAL_SURFACE ( 'NONE', #6895, 2.649999999999995914 ) ;
#7996 = ORIENTED_EDGE ( 'NONE', *, *, #3938, .F. ) ;
#7997 = CARTESIAN_POINT ( 'NONE',  ( 2.000000000000000000, 0.000000000000000000, 0.000000000000000000 ) ) ;
#7998 = ORIENTED_EDGE ( 'NONE', *, *, #572, .T. ) ;
#7999 = ORIENTED_EDGE ( 'NONE', *, *, #4889, .T. ) ;
#8000 = STYLED_ITEM ( 'NONE', ( #1720 ), #7232 ) ;
#8001 = LINE ( 'NONE', #6176, #3311 ) ;
#8002 = CARTESIAN_POINT ( 'NONE',  ( 23.61000000000001364, 0.000000000000000000, 0.000000000000000000 ) ) ;
#8003 = CARTESIAN_POINT ( 'NONE',  ( -31.74999999999995737, 0.000000000000000000, 2.000000000000000888 ) ) ;
#8004 = CARTESIAN_POINT ( 'NONE',  ( -3.103177678536665596, 6.291349734783570291, 8.006551011514465799 ) ) ;
#8005 = SURFACE_STYLE_USAGE ( .BOTH. , #320 ) ;
#8006 = CIRCLE ( 'NONE', #4445, 1.600000000000000311 ) ;
#8007 = ORIENTED_EDGE ( 'NONE', *, *, #5273, .T. ) ;
#8008 = EDGE_CURVE ( 'NONE', #3182, #7076, #5559, .T. ) ;
#8009 = ORIENTED_EDGE ( 'NONE', *, *, #457, .T. ) ;
#8010 = ORIENTED_EDGE ( 'NONE', *, *, #7516, .F. ) ;
#8011 = ADVANCED_FACE ( 'NONE', ( #4348 ), #1779, .T. ) ;
#8012 = PRODUCT_DEFINITION_SHAPE ( 'NONE', 'NONE',  #8218 ) ;
#8013 = ADVANCED_FACE ( 'NONE', ( #7549 ), #1239, .F. ) ;
#8014 = CARTESIAN_POINT ( 'NONE',  ( 2.000000000000000000, -1.773042676681340968, 2.059984127722458425E-15 ) ) ;
#8015 = FACE_OUTER_BOUND ( 'NONE', #6696, .T. ) ;
#8016 = LINE ( 'NONE', #327, #6881 ) ;
#8017 = EDGE_CURVE ( 'NONE', #5864, #5083, #6482, .T. ) ;
#8018 = UNCERTAINTY_MEASURE_WITH_UNIT (LENGTH_MEASURE( 1.000000000000000082E-05 ), #468, 'distance_accuracy_value', 'NONE');
#8019 = ORIENTED_EDGE ( 'NONE', *, *, #1350, .F. ) ;
#8020 = LINE ( 'NONE', #3592, #3945 ) ;
#8021 = EDGE_LOOP ( 'NONE', ( #7758, #6184 ) ) ;
#8022 = EDGE_LOOP ( 'NONE', ( #2120, #6864 ) ) ;
#8023 = FACE_OUTER_BOUND ( 'NONE', #3534, .T. ) ;
#8024 = CARTESIAN_POINT ( 'NONE',  ( 3.099999999999998757, 0.000000000000000000, 1.500000000000000222 ) ) ;
#8025 = LINE ( 'NONE', #4342, #7824 ) ;
#8026 = FACE_BOUND ( 'NONE', #4612, .T. ) ;
#8027 = ADVANCED_FACE ( 'NONE', ( #523 ), #1195, .F. ) ;
#8028 = ORIENTED_EDGE ( 'NONE', *, *, #5028, .T. ) ;
#8029 = EDGE_LOOP ( 'NONE', ( #1761, #2765 ) ) ;
#8030 = AXIS2_PLACEMENT_3D ( 'NONE', #1479, #4017, #7196 ) ;
#8031 = DIRECTION ( 'NONE',  ( 1.000000000000000000, 0.000000000000000000, 0.000000000000000000 ) ) ;
#8032 = DIRECTION ( 'NONE',  ( 0.000000000000000000, 0.000000000000000000, -1.000000000000000000 ) ) ;
#8033 = PLANE ( 'NONE',  #4775 ) ;
#8034 = CARTESIAN_POINT ( 'NONE',  ( -7.562723597472470821E-15, -3.402841154990142473E-15, 11.99999999999998934 ) ) ;
#8035 = TOROIDAL_SURFACE ( 'NONE', #5919, 2.700000000000000622, 0.2000000000000000111 ) ;
#8036 = CARTESIAN_POINT ( 'NONE',  ( 2.500000000000002220, 2.357898499370434386, -3.469446951953614189E-15 ) ) ;
#8037 = CIRCLE ( 'NONE', #1682, 2.149999999999999023 ) ;
#8038 = ORIENTED_EDGE ( 'NONE', *, *, #4204, .F. ) ;
#8039 = ORIENTED_EDGE ( 'NONE', *, *, #3973, .F. ) ;
#8040 = CARTESIAN_POINT ( 'NONE',  ( 0.2500000000000002220, 0.000000000000000000, 4.000000000000021316 ) ) ;
#8041 = CYLINDRICAL_SURFACE ( 'NONE', #898, 2.000000000000000888 ) ;
#8042 = DIRECTION ( 'NONE',  ( 1.000000000000000000, 0.000000000000000000, 0.000000000000000000 ) ) ;
#8043 = PLANE ( 'NONE',  #3348 ) ;
#8044 = DIRECTION ( 'NONE',  ( -0.000000000000000000, -0.000000000000000000, -1.000000000000000000 ) ) ;
#8045 = CARTESIAN_POINT ( 'NONE',  ( 4.199999999999995737, 2.449293598294707893E-16, -2.000000000000000888 ) ) ;
#8046 = EDGE_CURVE ( 'NONE', #2461, #7794, #6305, .T. ) ;
#8047 = AXIS2_PLACEMENT_3D ( 'NONE', #6921, #1905, #5146 ) ;
#8048 = ORIENTED_EDGE ( 'NONE', *, *, #3006, .T. ) ;
#8049 = EDGE_CURVE ( 'NONE', #4530, #2205, #3310, .T. ) ;
#8050 = TOROIDAL_SURFACE ( 'NONE', #2885, 3.299999999999999822, 0.2000000000000000111 ) ;
#8051 = ORIENTED_EDGE ( 'NONE', *, *, #1723, .F. ) ;
#8052 = EDGE_LOOP ( 'NONE', ( #1958, #2571, #323, #5132 ) ) ;
#8053 = PLANE ( 'NONE',  #5579 ) ;
#8054 = PLANE ( 'NONE',  #7820 ) ;
#8055 = DIRECTION ( 'NONE',  ( 0.000000000000000000, 0.000000000000000000, -1.000000000000000000 ) ) ;
#8056 = SURFACE_SIDE_STYLE ('',( #6245 ) ) ;
#8057 = PRODUCT_RELATED_PRODUCT_CATEGORY ( 'part', '', ( #2317 ) ) ;
#8058 = VECTOR ( 'NONE', #2074, 1000.000000000000000 ) ;
#8059 = EDGE_LOOP ( 'NONE', ( #3609, #1148, #2985, #6842 ) ) ;
#8060 = CARTESIAN_POINT ( 'NONE',  ( 2.000000000000000000, 1.773042676681340968, -2.276824562219559311E-15 ) ) ;
#8061 = ORIENTED_EDGE ( 'NONE', *, *, #556, .T. ) ;
#8062 = EDGE_LOOP ( 'NONE', ( #3336, #3283, #2987, #2437 ) ) ;
#8063 = VECTOR ( 'NONE', #1464, 1000.000000000000000 ) ;
#8064 = AXIS2_PLACEMENT_3D ( 'NONE', #4776, #2822, #7307 ) ;
#8065 = CONICAL_SURFACE ( 'NONE', #7931, 1.535500000000000087, 1.047197551196590748 ) ;
#8066 = CIRCLE ( 'NONE', #7544, 2.041999999999999815 ) ;
#8067 = DIRECTION ( 'NONE',  ( -0.000000000000000000, 1.000000000000000000, -0.000000000000000000 ) ) ;
#8068 = DIRECTION ( 'NONE',  ( 0.000000000000000000, 0.000000000000000000, -1.000000000000000000 ) ) ;
#8069 = EDGE_CURVE ( 'NONE', #1738, #6988, #6262, .T. ) ;
#8070 = CARTESIAN_POINT ( 'NONE',  ( -6.954591388923755169, -0.9174941424614954100, 8.033524818493585684 ) ) ;
#8071 = ADVANCED_FACE ( 'NONE', ( #3824 ), #7415, .T. ) ;
#8072 = AXIS2_PLACEMENT_3D ( 'NONE', #7677, #2039, #7055 ) ;
#8073 = CARTESIAN_POINT ( 'NONE',  ( -39.99999999999999289, 40.00000000000000711, 0.000000000000000000 ) ) ;
#8074 = CIRCLE ( 'NONE', #2644, 2.200000000000001066 ) ;
#8075 = AXIS2_PLACEMENT_3D ( 'NONE', #2852, #4222, #5393 ) ;
#8076 = ORIENTED_EDGE ( 'NONE', *, *, #1684, .T. ) ;
#8077 = VERTEX_POINT ( 'NONE', #8161 ) ;
#8078 = AXIS2_PLACEMENT_3D ( 'NONE', #2352, #1107, #7375 ) ;
#8079 = EDGE_CURVE ( 'NONE', #3458, #4267, #8126, .T. ) ;
#8080 = CARTESIAN_POINT ( 'NONE',  ( 55.00000000000000000, -8.000000000000001776, 15.50000000000000355 ) ) ;
#8081 = AXIS2_PLACEMENT_3D ( 'NONE', #2131, #830, #2058 ) ;
#8082 = DIRECTION ( 'NONE',  ( -0.000000000000000000, -0.000000000000000000, 1.000000000000000000 ) ) ;
#8083 = CARTESIAN_POINT ( 'NONE',  ( 1.274374112546295138E-14, 85.00000000000017053, 2.000000000000043521 ) ) ;
#8084 = DIRECTION ( 'NONE',  ( -0.000000000000000000, -0.000000000000000000, 1.000000000000000000 ) ) ;
#8085 = AXIS2_PLACEMENT_3D ( 'NONE', #5304, #924, #3382 ) ;
#8086 = AXIS2_PLACEMENT_3D ( 'NONE', #7722, #3912, #2076 ) ;
#8087 = CARTESIAN_POINT ( 'NONE',  ( 30.00000000000001066, -29.99999999999997868, 10.00000000000000000 ) ) ;
#8088 = CARTESIAN_POINT ( 'NONE',  ( 55.00000000000000000, -10.00000000000000000, 15.50000000000000355 ) ) ;
#8089 = PRODUCT ( 'socket head cap screw_iso_ISO 4762 M5 x 25 - 25N', 'socket head cap screw_iso_ISO 4762 M5 x 25 - 25N', '', ( #3457 ) ) ;
#8090 = ORIENTED_EDGE ( 'NONE', *, *, #148, .F. ) ;
#8091 = CIRCLE ( 'NONE', #384, 2.600000000000000089 ) ;
#8092 = ORIENTED_EDGE ( 'NONE', *, *, #6865, .F. ) ;
#8093 = CARTESIAN_POINT ( 'NONE',  ( 2.000000000000000000, -0.8865213383406721492, -1.535499999999998977 ) ) ;
#8094 = CARTESIAN_POINT ( 'NONE',  ( 2.681483223904246316, -3.070647092368468112, -2.699999999999980194 ) ) ;
#8095 = DIRECTION ( 'NONE',  ( -0.8191520442889896891, 0.000000000000000000, -0.5735764363510490460 ) ) ;
#8096 = CARTESIAN_POINT ( 'NONE',  ( -4.000000000000000000, 2.309401076758531346, -2.342734410091827701 ) ) ;
#8097 = CARTESIAN_POINT ( 'NONE',  ( 2.000000000000000000, -0.8865213383406690406, 1.535500000000000975 ) ) ;
#8098 = CARTESIAN_POINT ( 'NONE',  ( 2.500000000000002220, 2.357898499370434386, -3.469446951953614189E-15 ) ) ;
#8099 = STYLED_ITEM ( 'NONE', ( #6563 ), #1426 ) ;
#8100 = VERTEX_POINT ( 'NONE', #7465 ) ;
#8101 = AXIS2_PLACEMENT_3D ( 'NONE', #728, #3943, #3868 ) ;
#8102 = ORIENTED_EDGE ( 'NONE', *, *, #5445, .F. ) ;
#8103 = ORIENTED_EDGE ( 'NONE', *, *, #5860, .T. ) ;
#8104 = VERTEX_POINT ( 'NONE', #3154 ) ;
#8105 = CARTESIAN_POINT ( 'NONE',  ( 2.500000000000002220, -1.178949249685215417, 2.042000000000002036 ) ) ;
#8106 = DIRECTION ( 'NONE',  ( -1.000000000000000000, 0.000000000000000000, 0.000000000000000000 ) ) ;
#8107 = EDGE_CURVE ( 'NONE', #1171, #4324, #2538, .T. ) ;
#8108 = ADVANCED_FACE ( 'NONE', ( #4309 ), #6611, .F. ) ;
#8109 = VERTEX_POINT ( 'NONE', #5686 ) ;
#8110 = CARTESIAN_POINT ( 'NONE',  ( 0.000000000000000000, 0.000000000000000000, 0.000000000000000000 ) ) ;
#8111 = EDGE_LOOP ( 'NONE', ( #2616, #123, #3018, #777 ) ) ;
#8112 = ORIENTED_EDGE ( 'NONE', *, *, #5300, .F. ) ;
#8113 = DIRECTION ( 'NONE',  ( 0.000000000000000000, 0.000000000000000000, -1.000000000000000000 ) ) ;
#8114 = CARTESIAN_POINT ( 'NONE',  ( -41.98843075541677194, 84.00772803575827652, -2.189015531277937132 ) ) ;
#8115 = AXIS2_PLACEMENT_3D ( 'NONE', #6179, #7477, #4993 ) ;
#8116 = DIRECTION ( 'NONE',  ( -1.000000000000000000, 0.000000000000000000, 0.000000000000000000 ) ) ;
#8117 = DIRECTION ( 'NONE',  ( 1.000000000000000000, 0.000000000000000000, 0.000000000000000000 ) ) ;
#8118 = CIRCLE ( 'NONE', #2690, 2.500000000000000444 ) ;
#8119 = EDGE_CURVE ( 'NONE', #2900, #5567, #239, .T. ) ;
#8120 = EDGE_CURVE ( 'NONE', #4437, #191, #6501, .T. ) ;
#8121 = VERTEX_POINT ( 'NONE', #7166 ) ;
#8122 = ORIENTED_EDGE ( 'NONE', *, *, #7764, .F. ) ;
#8123 = EDGE_CURVE ( 'NONE', #6551, #3168, #2574, .T. ) ;
#8124 = CARTESIAN_POINT ( 'NONE',  ( -60.00000000000000000, 10.00000000000000000, 10.50000000000000000 ) ) ;
#8125 = DIRECTION ( 'NONE',  ( -0.000000000000000000, -0.000000000000000000, -1.000000000000000000 ) ) ;
#8126 = LINE ( 'NONE', #6344, #2773 ) ;
#8127 = CARTESIAN_POINT ( 'NONE',  ( 7.000000000000000000, 8.572527594031473190E-16, 0.000000000000000000 ) ) ;
#8128 = LINE ( 'NONE', #5027, #5305 ) ;
#8129 = DIRECTION ( 'NONE',  ( -0.000000000000000000, -0.000000000000000000, -1.000000000000000000 ) ) ;
#8130 = ORIENTED_EDGE ( 'NONE', *, *, #2301, .F. ) ;
#8131 = ORIENTED_EDGE ( 'NONE', *, *, #3063, .T. ) ;
#8132 = DIRECTION ( 'NONE',  ( 0.000000000000000000, 0.4999999999999991118, -0.8660254037844391517 ) ) ;
#8133 = DIRECTION ( 'NONE',  ( 0.000000000000000000, 0.4999999999999990008, -0.8660254037844391517 ) ) ;
#8134 = DIRECTION ( 'NONE',  ( 1.000000000000000000, 0.000000000000000000, 0.000000000000000000 ) ) ;
#8135 = DIRECTION ( 'NONE',  ( 0.000000000000000000, -0.000000000000000000, -1.000000000000000000 ) ) ;
#8136 = CARTESIAN_POINT ( 'NONE',  ( -60.00000000000000000, 10.00000000000000000, 20.00000000000000355 ) ) ;
#8137 = DIRECTION ( 'NONE',  ( 0.000000000000000000, -0.5000000000000011102, -0.8660254037844379305 ) ) ;
#8138 = EDGE_LOOP ( 'NONE', ( #1836, #1540 ) ) ;
#8139 = VERTEX_POINT ( 'NONE', #5263 ) ;
#8140 = ORIENTED_EDGE ( 'NONE', *, *, #4842, .F. ) ;
#8141 = EDGE_CURVE ( 'NONE', #6378, #4688, #5230, .T. ) ;
#8142 = VERTEX_POINT ( 'NONE', #177 ) ;
#8143 = FACE_OUTER_BOUND ( 'NONE', #2381, .T. ) ;
#8144 = LINE ( 'NONE', #6324, #766 ) ;
#8145 = ADVANCED_FACE ( 'NONE', ( #98 ), #1482, .F. ) ;
#8146 = ORIENTED_EDGE ( 'NONE', *, *, #4393, .F. ) ;
#8147 = DIRECTION ( 'NONE',  ( 0.000000000000000000, 1.000000000000000000, 0.000000000000000000 ) ) ;
#8148 = VERTEX_POINT ( 'NONE', #5915 ) ;
#8149 = CIRCLE ( 'NONE', #6158, 1.535500000000000087 ) ;
#8150 = ORIENTED_EDGE ( 'NONE', *, *, #2023, .F. ) ;
#8151 = DIRECTION ( 'NONE',  ( -0.000000000000000000, -0.000000000000000000, 1.000000000000000000 ) ) ;
#8152 = CARTESIAN_POINT ( 'NONE',  ( -41.97904239022134476, 83.67335008385822448, 2.000000000000043521 ) ) ;
#8153 = DIRECTION ( 'NONE',  ( 0.000000000000000000, 1.000000000000000000, -9.783878858594330870E-16 ) ) ;
#8154 = CARTESIAN_POINT ( 'NONE',  ( -5.566961118109779783, -4.268296125650788753, 8.021439803987641781 ) ) ;
#8155 = CARTESIAN_POINT ( 'NONE',  ( 0.4618352976297687151, 6.999999999999993783, 8.000000000000024869 ) ) ;
#8156 = EDGE_CURVE ( 'NONE', #7658, #6819, #4904, .T. ) ;
#8157 = ADVANCED_FACE ( 'NONE', ( #6532 ), #842, .F. ) ;
#8158 = EDGE_LOOP ( 'NONE', ( #2791, #72, #2874 ) ) ;
#8159 = EDGE_LOOP ( 'NONE', ( #4678, #1022, #5832, #5792 ) ) ;
#8160 = DIRECTION ( 'NONE',  ( -1.000000000000000000, 0.000000000000000000, 0.000000000000000000 ) ) ;
#8161 = CARTESIAN_POINT ( 'NONE',  ( -58.00000000000006395, 7.999999999999996447, 11.99999999999998934 ) ) ;
#8162 = DIRECTION ( 'NONE',  ( -1.000000000000000000, 0.000000000000000000, 0.000000000000000000 ) ) ;
#8163 = LINE ( 'NONE', #3742, #2913 ) ;
#8164 = EDGE_CURVE ( 'NONE', #910, #3954, #2905, .T. ) ;
#8165 = DIRECTION ( 'NONE',  ( -0.000000000000000000, 1.000000000000000000, -0.000000000000000000 ) ) ;
#8166 = ORIENTED_EDGE ( 'NONE', *, *, #2744, .T. ) ;
#8167 = DIRECTION ( 'NONE',  ( 1.412205397084881070E-17, -2.775557561562891967E-17, -1.000000000000000000 ) ) ;
#8168 = CARTESIAN_POINT ( 'NONE',  ( -27.35000000000000497, -29.99999999999999289, 1.734723475976807094E-15 ) ) ;
#8169 = DIRECTION ( 'NONE',  ( -0.000000000000000000, -0.000000000000000000, 1.000000000000000000 ) ) ;
#8170 = FACE_OUTER_BOUND ( 'NONE', #882, .T. ) ;
#8171 = DIRECTION ( 'NONE',  ( 2.168404344971008621E-16, -1.000000000000000000, 0.000000000000000000 ) ) ;
#8172 = CARTESIAN_POINT ( 'NONE',  ( 49.94313152867115235, 87.38422970439145843, 0.3160888171753749032 ) ) ;
#8173 = CIRCLE ( 'NONE', #6715, 2.500000000000002220 ) ;
#8174 = VECTOR ( 'NONE', #6220, 1000.000000000000114 ) ;
#8175 = VERTEX_POINT ( 'NONE', #3271 ) ;
#8176 = ORIENTED_EDGE ( 'NONE', *, *, #179, .F. ) ;
#8177 = CARTESIAN_POINT ( 'NONE',  ( 0.000000000000000000, -1.773042676681340524, 1.734723475976807094E-15 ) ) ;
#8178 = ORIENTED_EDGE ( 'NONE', *, *, #8119, .T. ) ;
#8179 = ORIENTED_EDGE ( 'NONE', *, *, #271, .F. ) ;
#8180 = PLANE ( 'NONE',  #6207 ) ;
#8182 = EDGE_CURVE ( 'NONE', #708, #6538, #4479, .T. ) ;
#8181 = LINE ( 'NONE', #6323, #6495 ) ;
#8183 = DIRECTION ( 'NONE',  ( 1.000000000000000000, 0.000000000000000000, 0.000000000000000000 ) ) ;
#8184 = VERTEX_POINT ( 'NONE', #7004 ) ;
#8185 = CARTESIAN_POINT ( 'NONE',  ( 49.97498335796547053, 83.41456698278581428, 1.808729786019549923 ) ) ;
#8186 = ORIENTED_EDGE ( 'NONE', *, *, #6057, .T. ) ;
#8187 = EDGE_LOOP ( 'NONE', ( #2089, #1133, #3804 ) ) ;
#8188 = AXIS2_PLACEMENT_3D ( 'NONE', #2060, #6526, #7156 ) ;
#8189 = CARTESIAN_POINT ( 'NONE',  ( 0.000000000000000000, 0.000000000000000000, 10.00000000000000000 ) ) ;
#8190 = CARTESIAN_POINT ( 'NONE',  ( 41.94398068067085461, 87.17027663518501868, 1.056300034359340723 ) ) ;
#8191 = CYLINDRICAL_SURFACE ( 'NONE', #7787, 2.650000000000002576 ) ;
#8192 = AXIS2_PLACEMENT_3D ( 'NONE', #1192, #6793, #3780 ) ;
#8193 = FILL_AREA_STYLE ('',( #3098 ) ) ;
#8194 = CARTESIAN_POINT ( 'NONE',  ( 9.020562060468115204E-14, -7.000000000000000000, 7.999999999999977796 ) ) ;
#8195 = STYLED_ITEM ( 'NONE', ( #5407 ), #3934 ) ;
#8196 = PLANE ( 'NONE',  #3482 ) ;
#8197 = AXIS2_PLACEMENT_3D ( 'NONE', #7788, #5208, #5316 ) ;
#8198 = AXIS2_PLACEMENT_3D ( 'NONE', #6105, #408, #1833 ) ;
#8199 = ORIENTED_EDGE ( 'NONE', *, *, #3860, .F. ) ;
#8200 = VERTEX_POINT ( 'NONE', #2031 ) ;
#8201 = CARTESIAN_POINT ( 'NONE',  ( 4.000000000000003553, -0.3902508023145563332, -1.980363030680554193E-15 ) ) ;
#8202 = DIRECTION ( 'NONE',  ( 0.000000000000000000, 0.000000000000000000, -1.000000000000000000 ) ) ;
#8203 = DIRECTION ( 'NONE',  ( 1.000000000000000000, 0.000000000000000000, 0.000000000000000000 ) ) ;
#8204 = EDGE_CURVE ( 'NONE', #939, #7330, #7148, .T. ) ;
#8205 = AXIS2_PLACEMENT_3D ( 'NONE', #7029, #677, #5051 ) ;
#8206 = NEXT_ASSEMBLY_USAGE_OCCURRENCE ( 'NAUO1', ' ', ' ', #7571, #1782, $ ) ;
#8207 = NEXT_ASSEMBLY_USAGE_OCCURRENCE ( 'NAUO2', ' ', ' ', #7571, #5748, $ ) ;
#8208 = NEXT_ASSEMBLY_USAGE_OCCURRENCE ( 'NAUO3', ' ', ' ', #7571, #6186, $ ) ;
#8209 = NEXT_ASSEMBLY_USAGE_OCCURRENCE ( 'NAUO4', ' ', ' ', #7571, #1427, $ ) ;
#8210 = NEXT_ASSEMBLY_USAGE_OCCURRENCE ( 'NAUO5', ' ', ' ', #7571, #7899, $ ) ;
#8211 = NEXT_ASSEMBLY_USAGE_OCCURRENCE ( 'NAUO6', ' ', ' ', #7571, #6186, $ ) ;
#8212 = NEXT_ASSEMBLY_USAGE_OCCURRENCE ( 'NAUO7', ' ', ' ', #7571, #7899, $ ) ;
#8213 = NEXT_ASSEMBLY_USAGE_OCCURRENCE ( 'NAUO8', ' ', ' ', #7571, #7899, $ ) ;
#8214 = NEXT_ASSEMBLY_USAGE_OCCURRENCE ( 'NAUO9', ' ', ' ', #7571, #2790, $ ) ;
#8215 = NEXT_ASSEMBLY_USAGE_OCCURRENCE ( 'NAUO10', ' ', ' ', #7571, #2283, $ ) ;
#8216 = NEXT_ASSEMBLY_USAGE_OCCURRENCE ( 'NAUO11', ' ', ' ', #7571, #2283, $ ) ;
#8217 = NEXT_ASSEMBLY_USAGE_OCCURRENCE ( 'NAUO12', ' ', ' ', #7571, #2884, $ ) ;
#8218 = NEXT_ASSEMBLY_USAGE_OCCURRENCE ( 'NAUO13', ' ', ' ', #7571, #7665, $ ) ;
#8219 = NEXT_ASSEMBLY_USAGE_OCCURRENCE ( 'NAUO14', ' ', ' ', #7571, #7665, $ ) ;
#8220 = NEXT_ASSEMBLY_USAGE_OCCURRENCE ( 'NAUO15', ' ', ' ', #7571, #1328, $ ) ;
#8221 = NEXT_ASSEMBLY_USAGE_OCCURRENCE ( 'NAUO16', ' ', ' ', #7571, #2884, $ ) ;
#8222 = NEXT_ASSEMBLY_USAGE_OCCURRENCE ( 'NAUO17', ' ', ' ', #7571, #2884, $ ) ;
ENDSEC;
END-ISO-10303-21;
